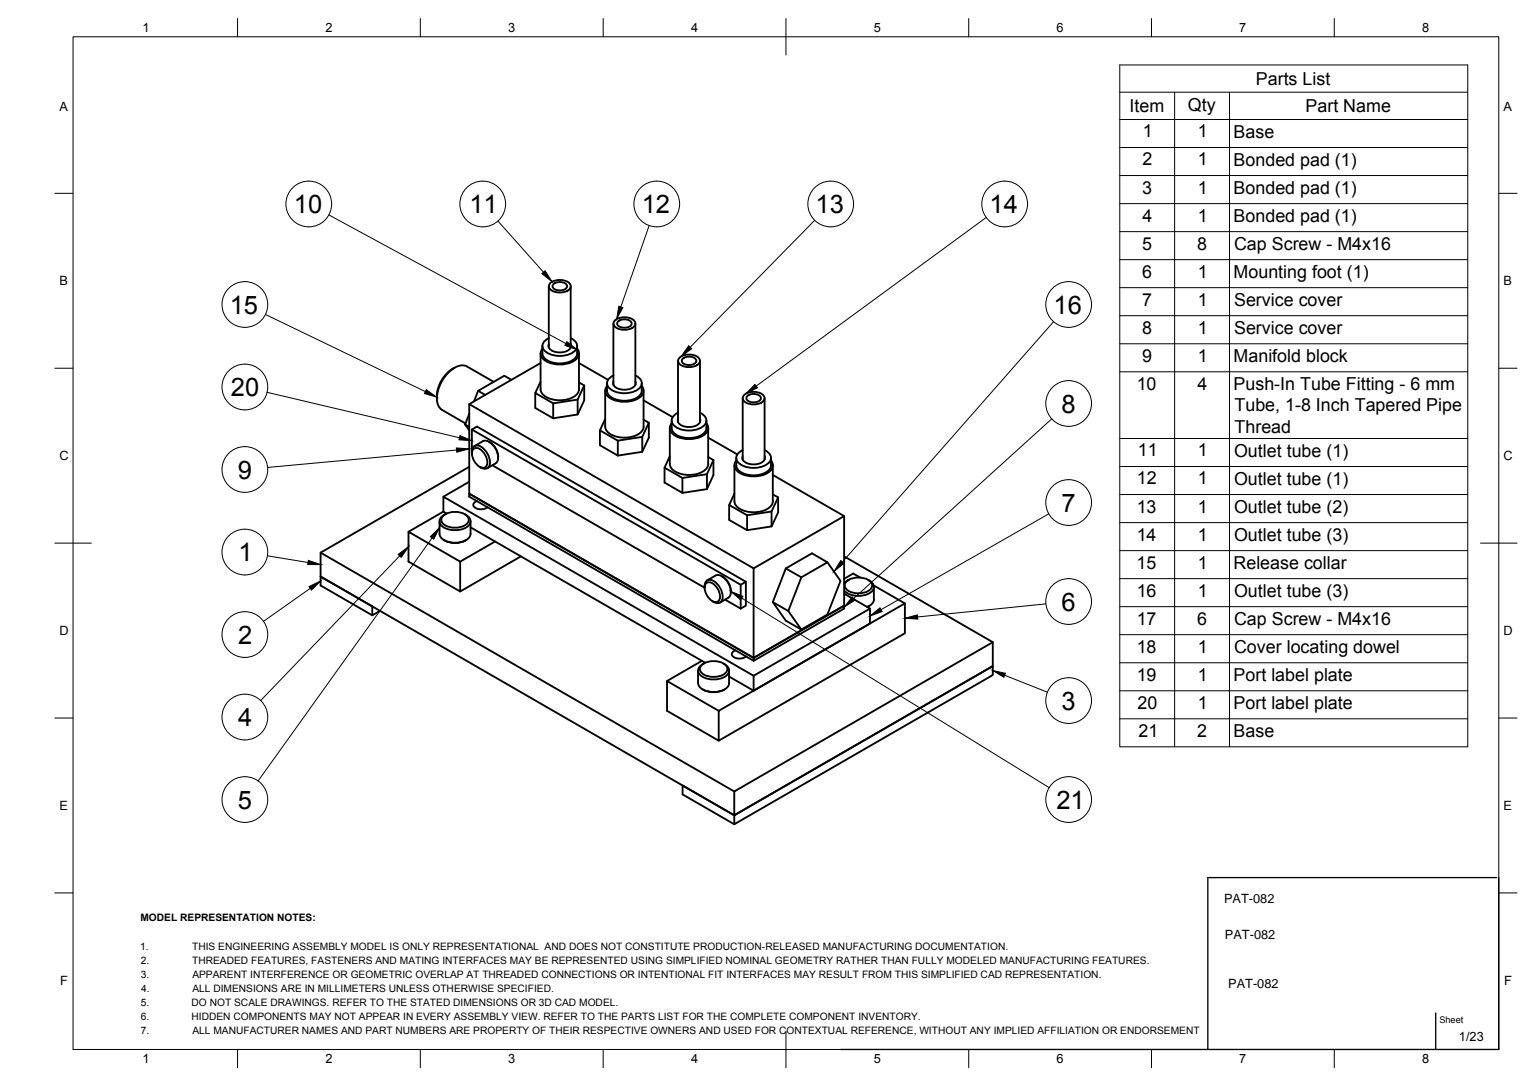
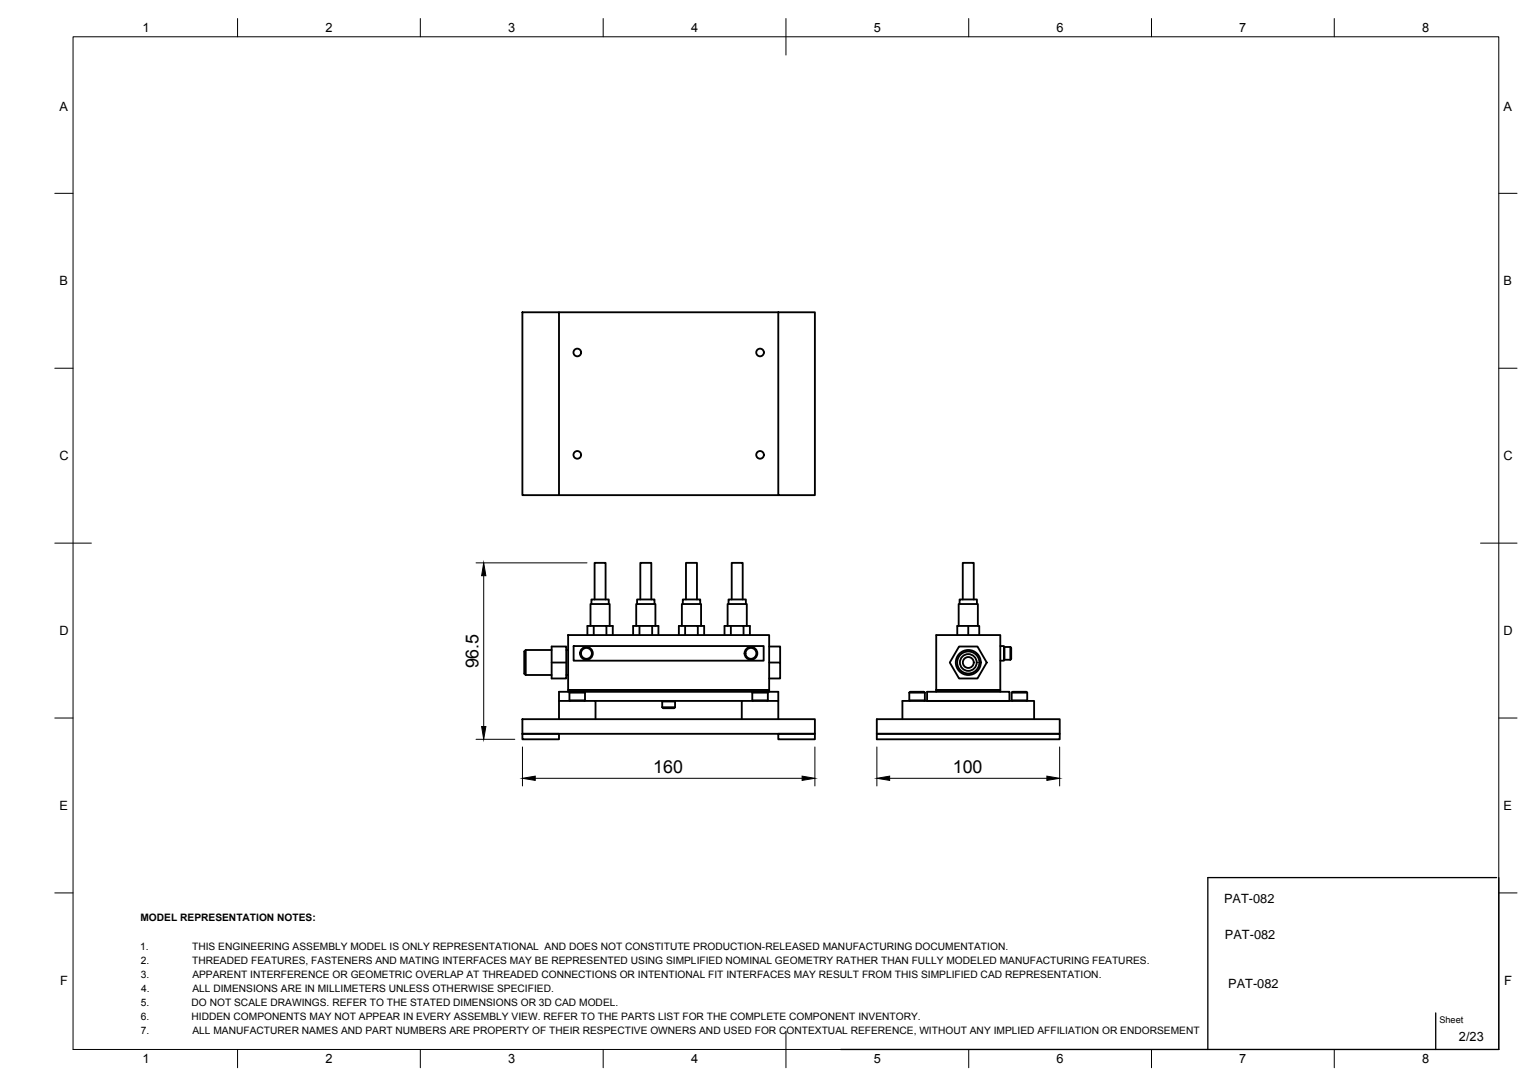
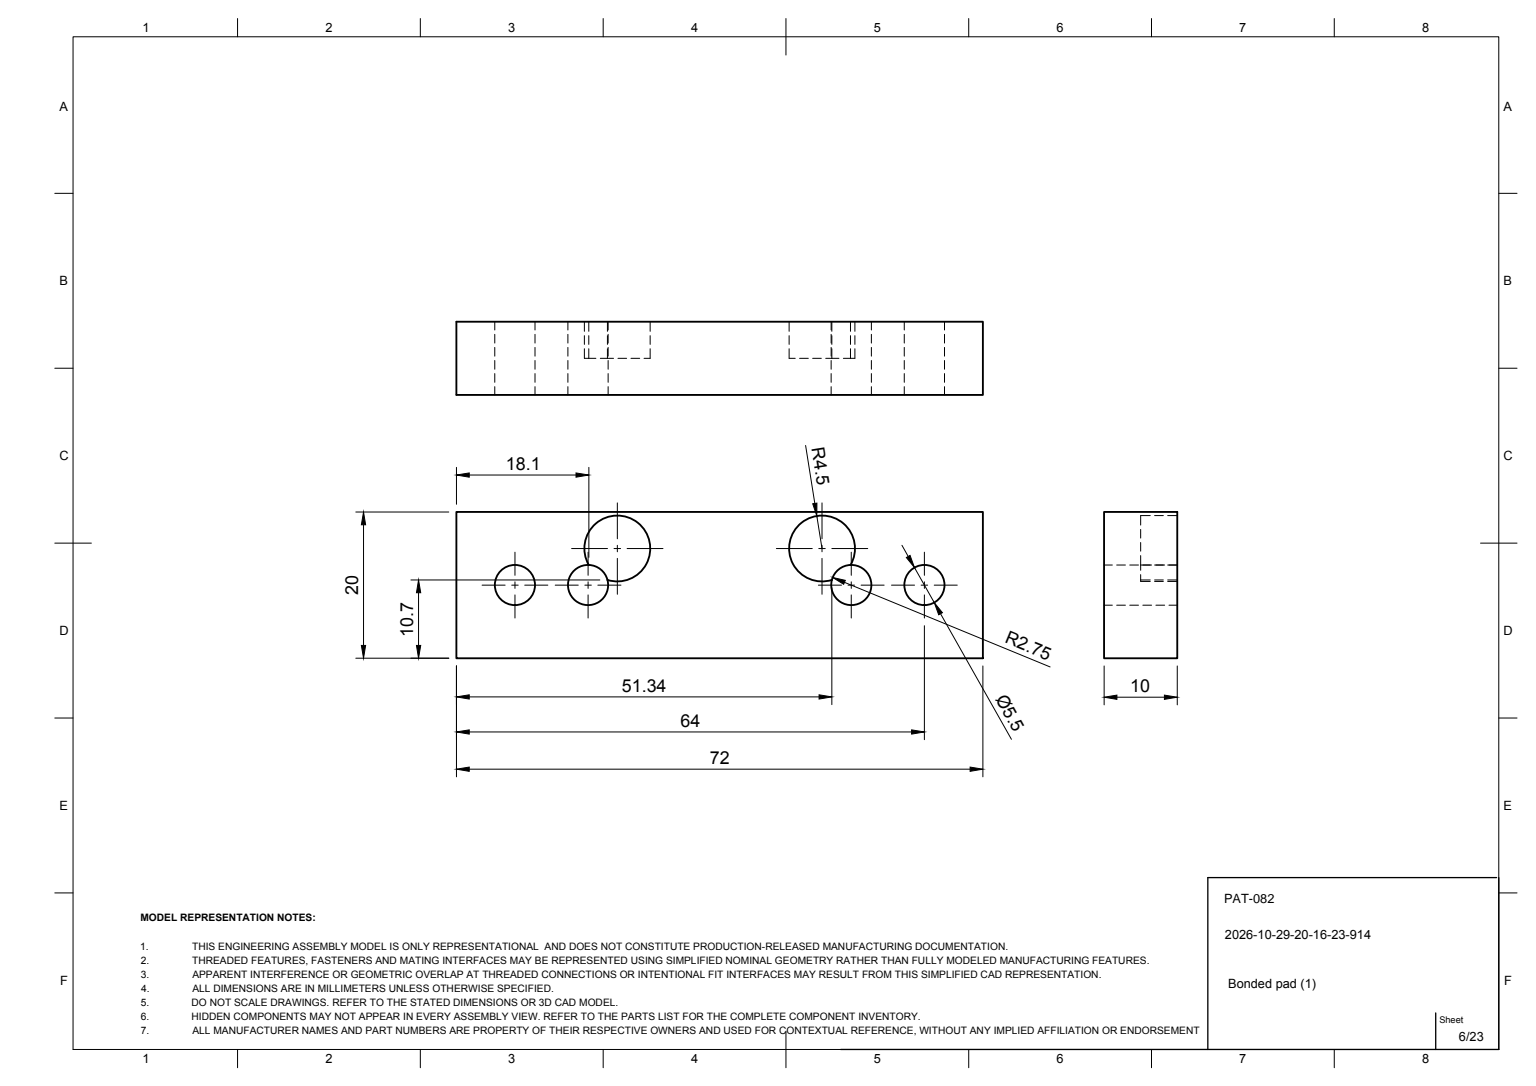
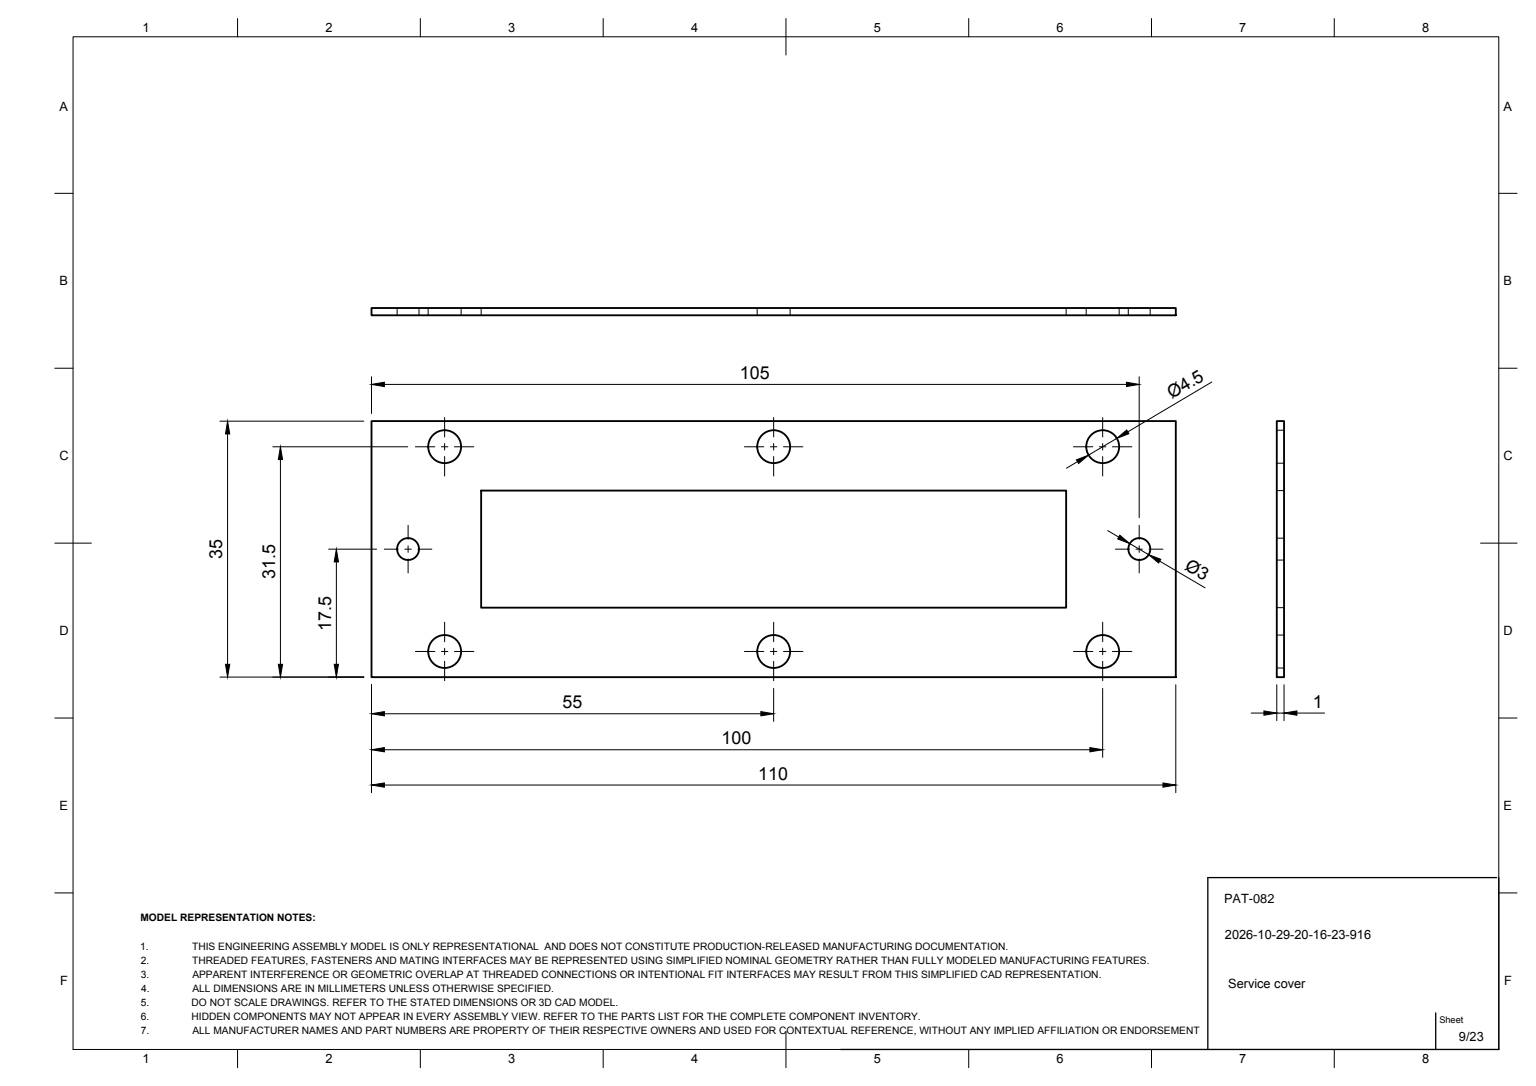
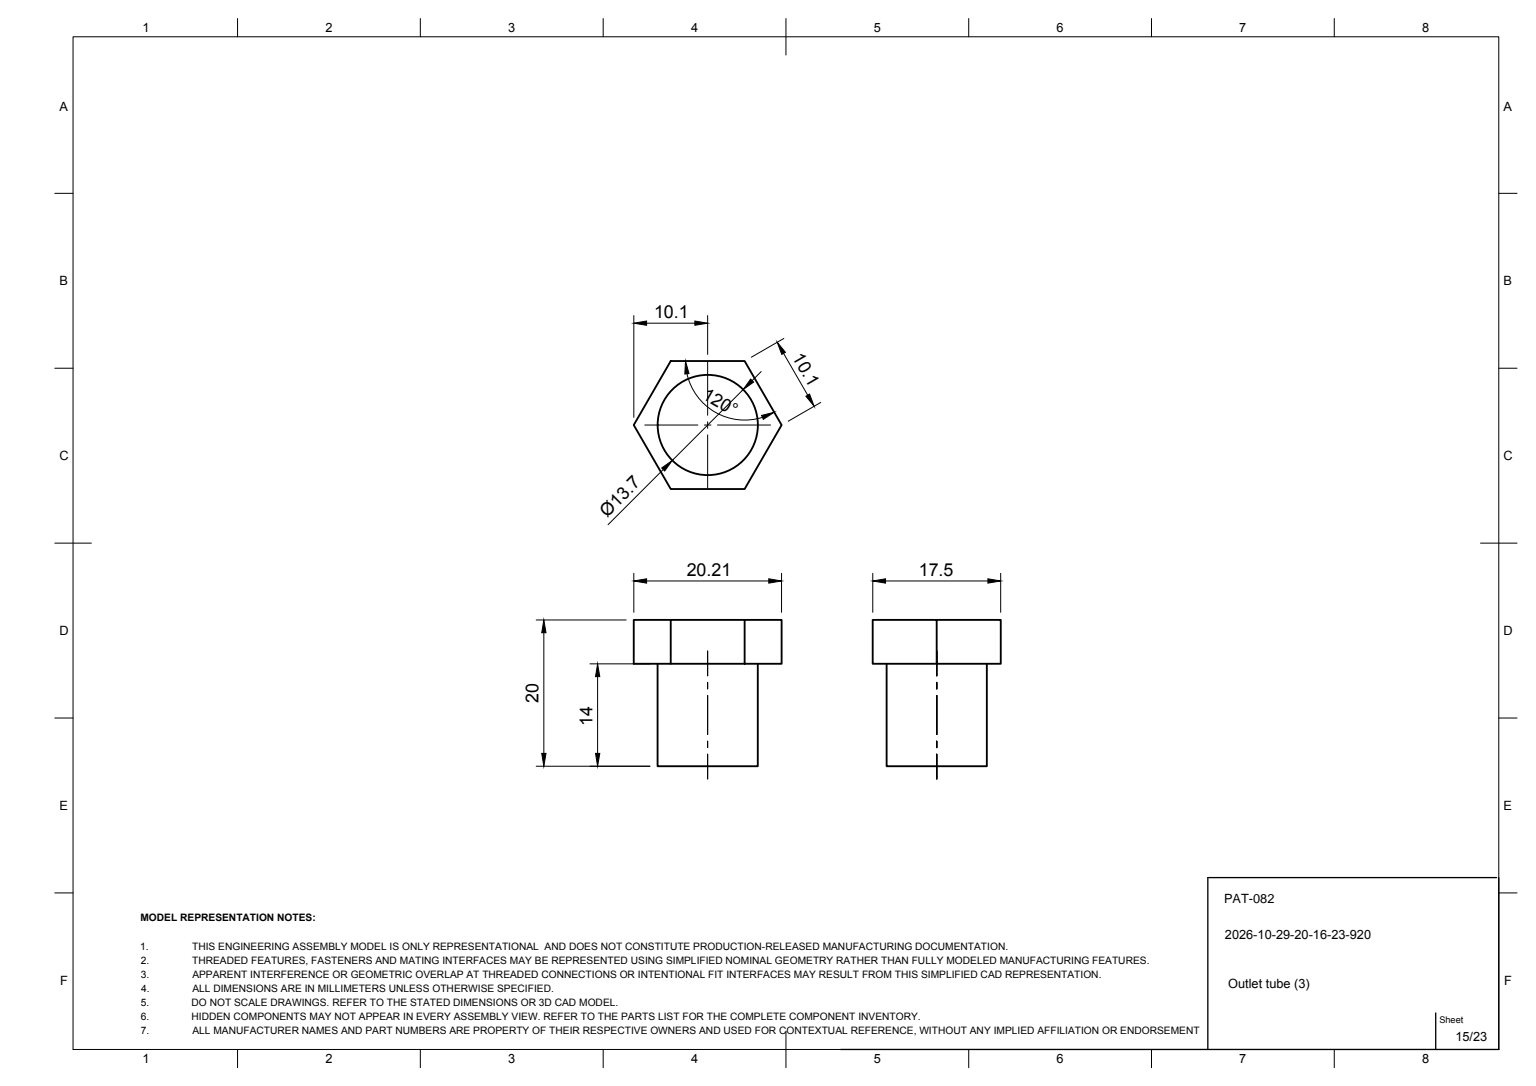
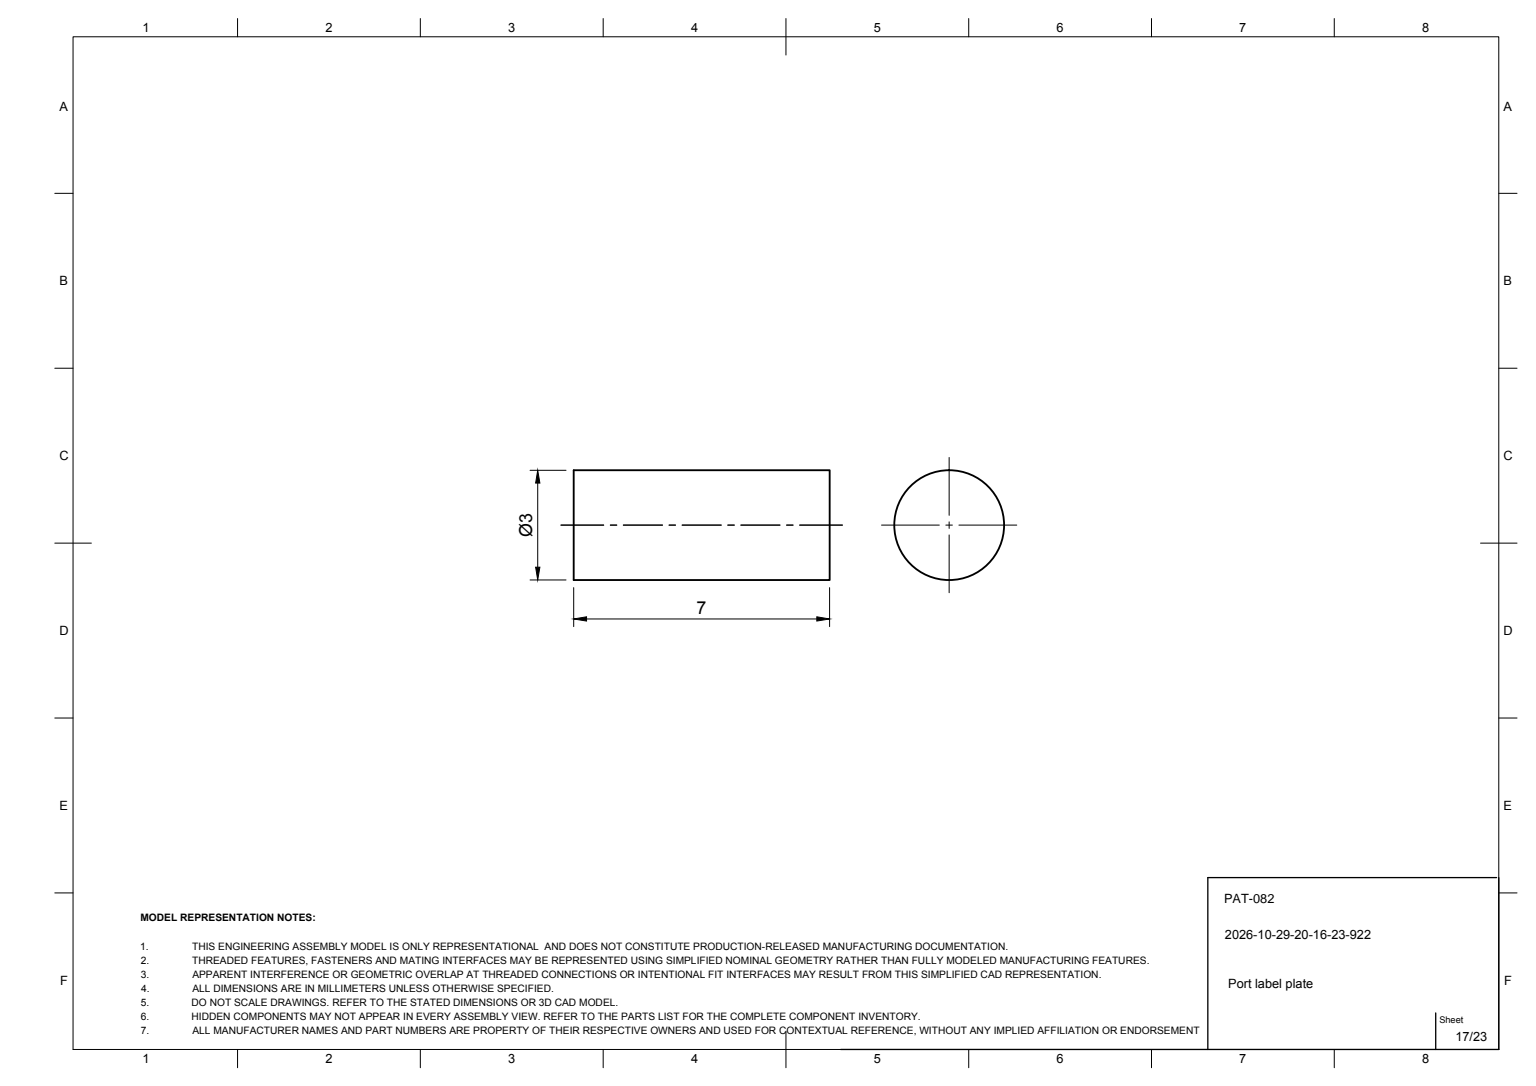
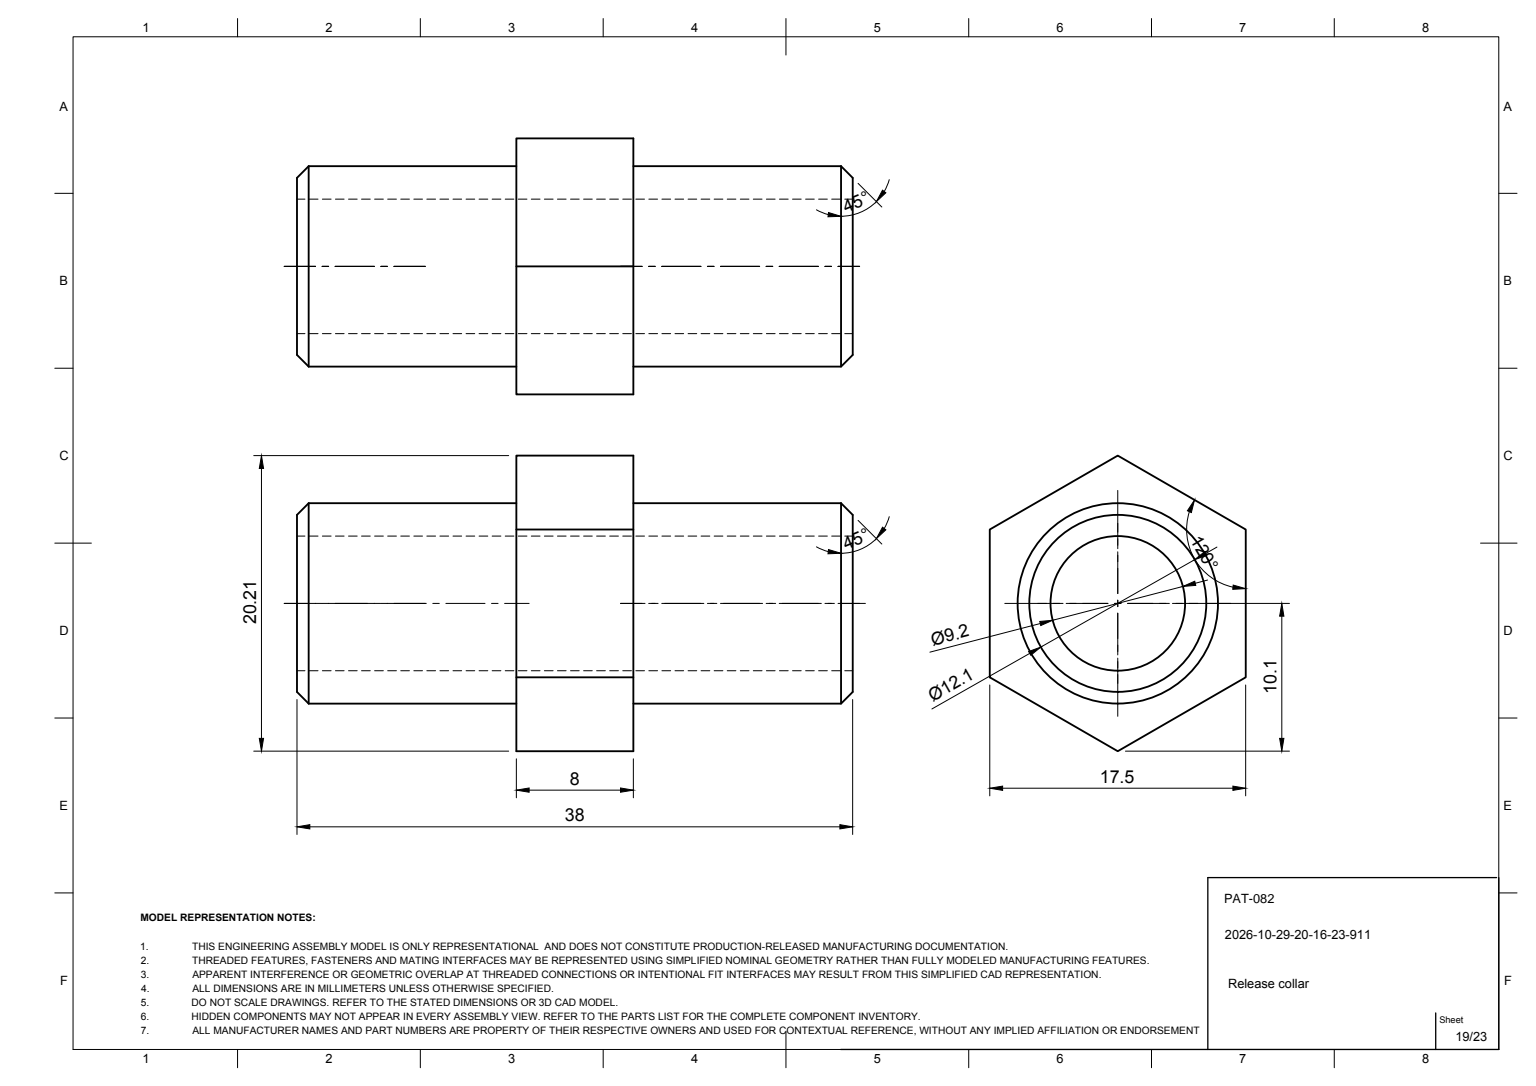
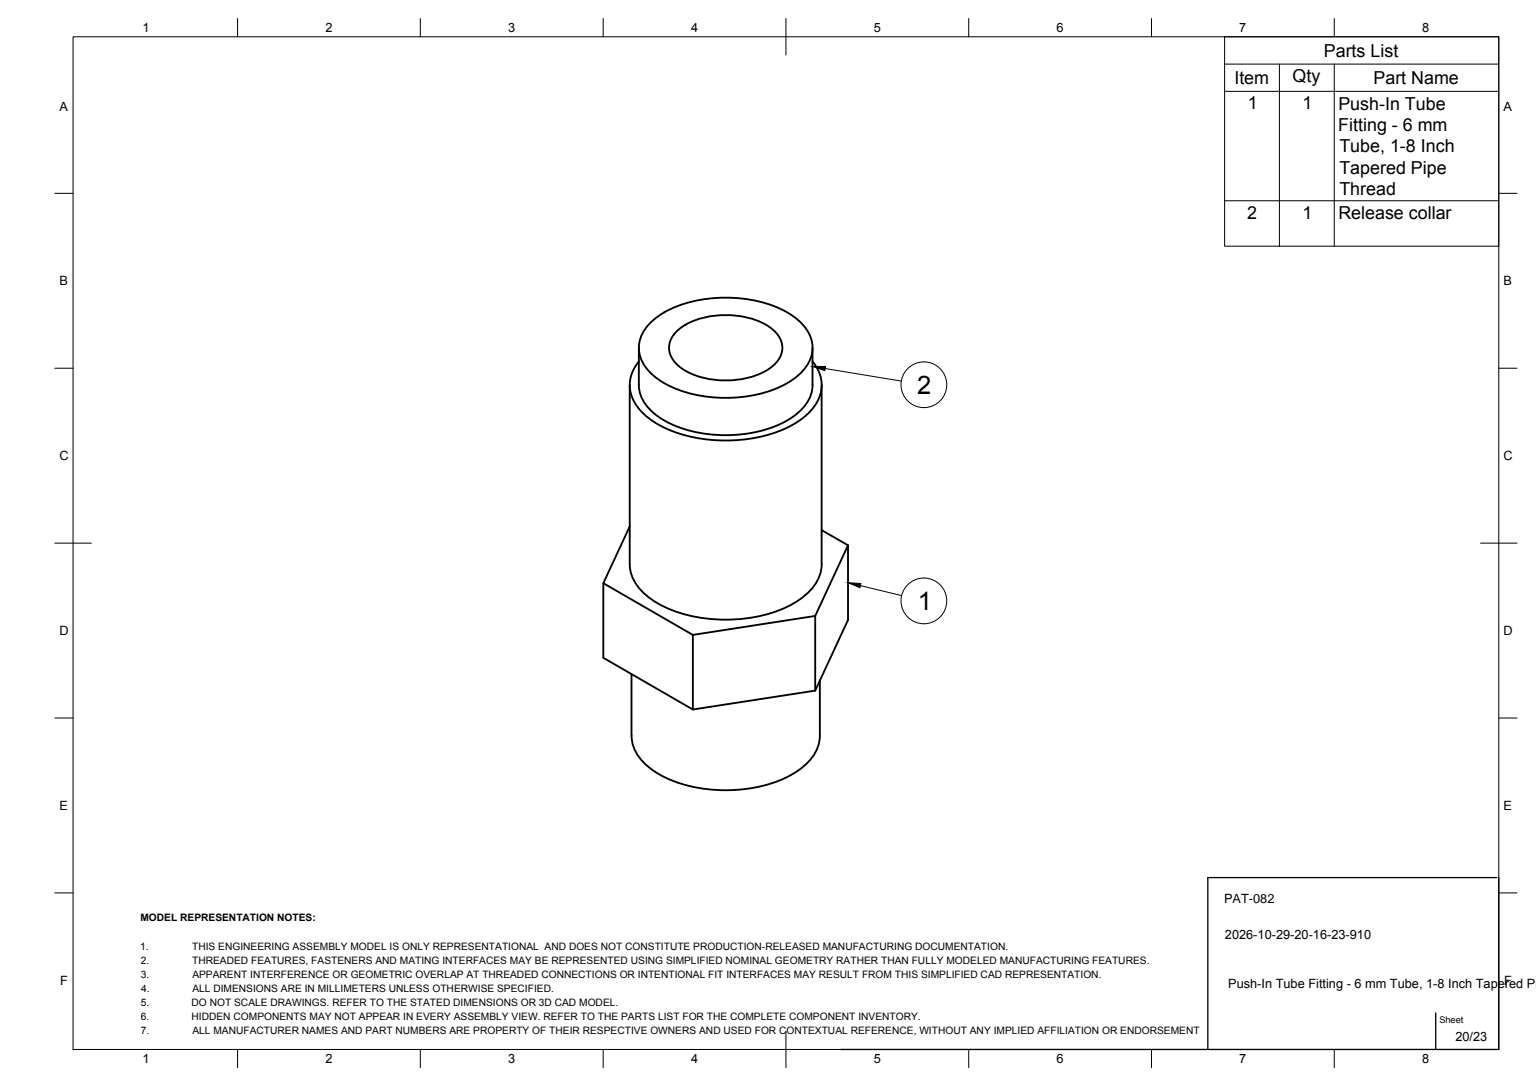
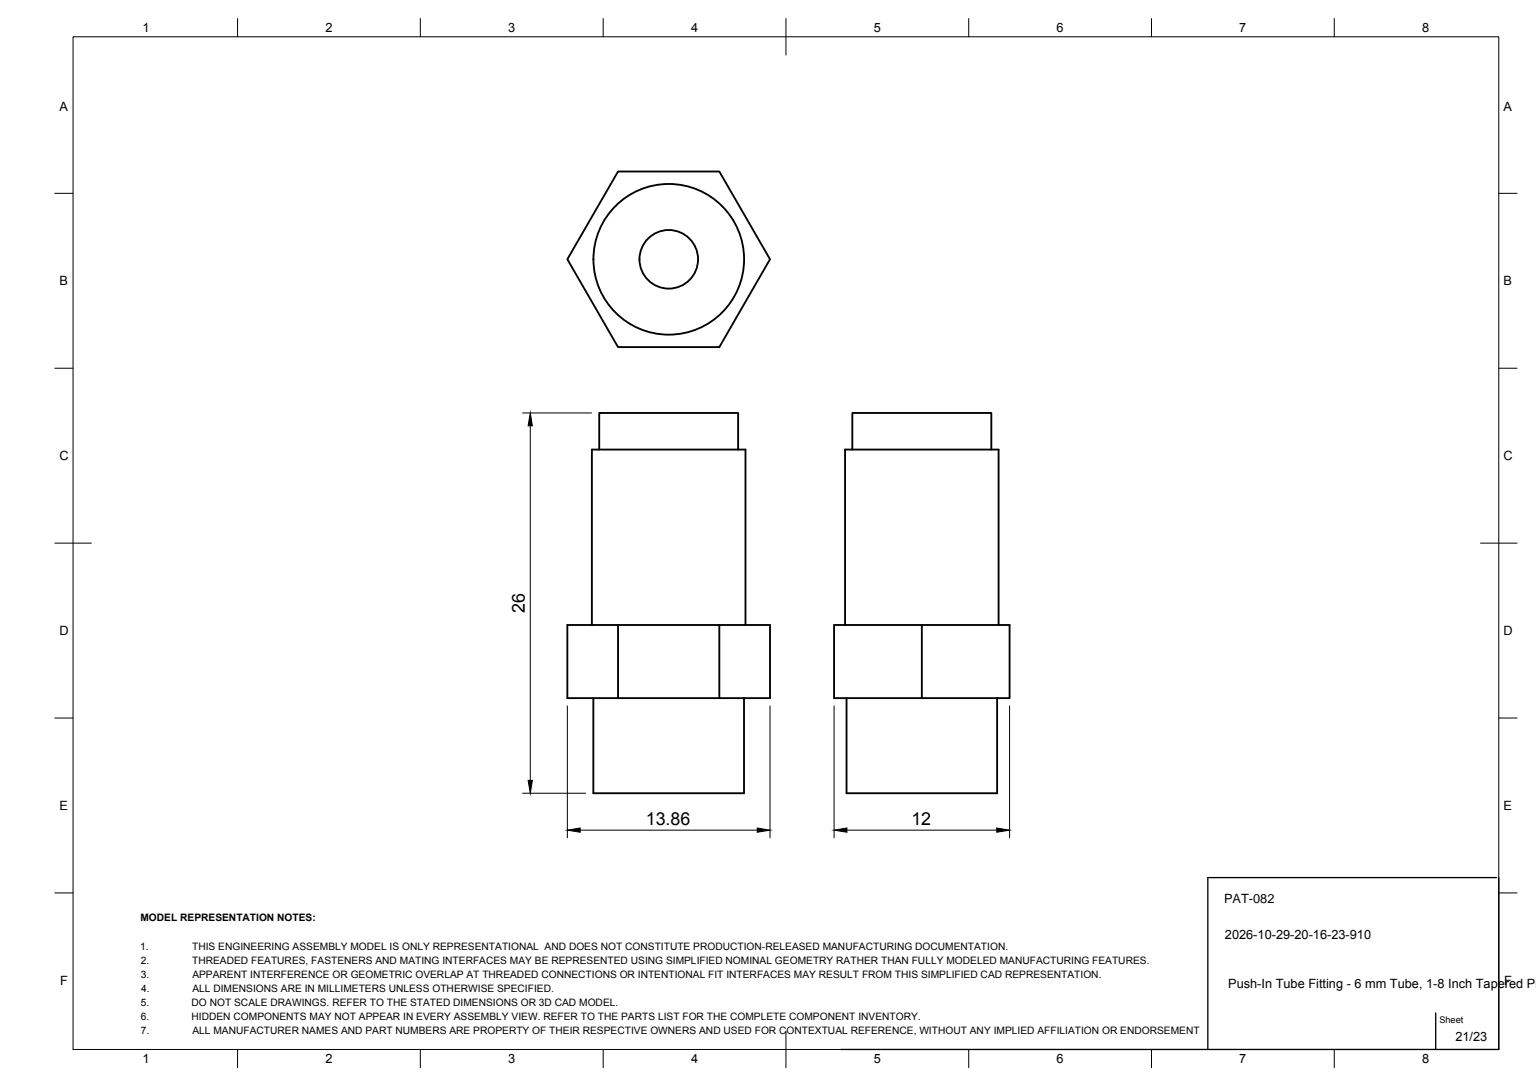
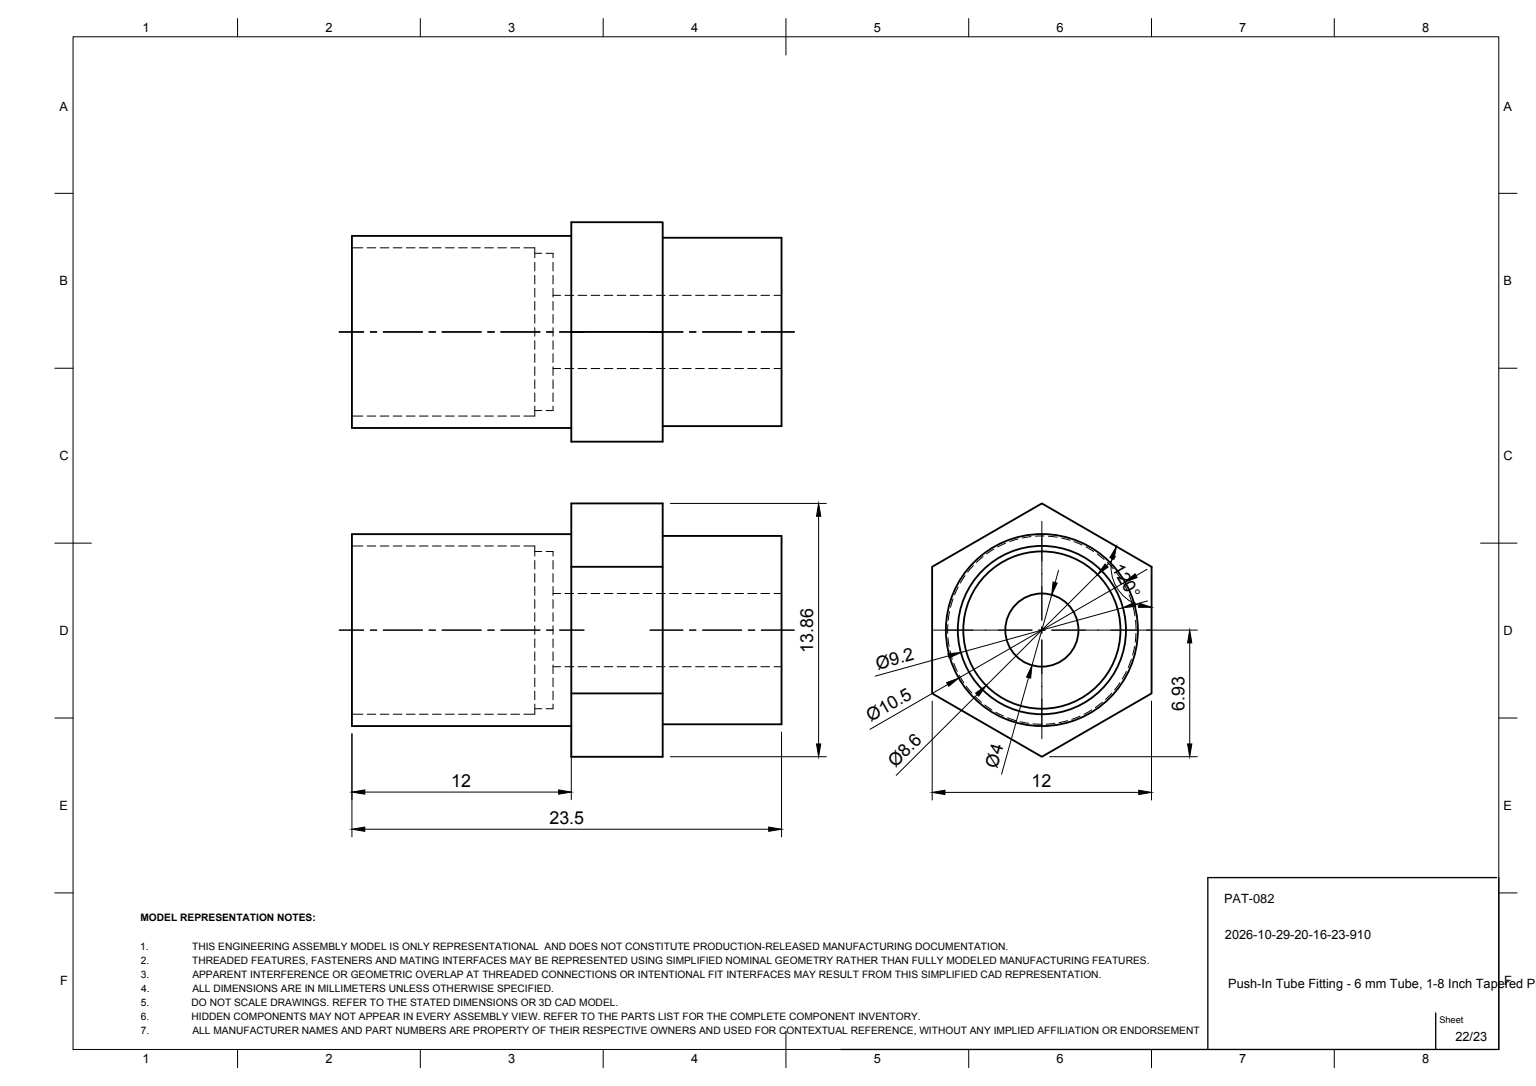
ISO-10303-21;
HEADER;
/* Generated by software containing ST-Developer
 * from STEP Tools, Inc. (www.steptools.com) 
 */

FILE_DESCRIPTION(
/* description */ ('PAT-082'),
/* implementation_level */ '2;1');

FILE_NAME(
/* name */ 'PAT-082',
/* time_stamp */ '2026-10-29T20:16:13-07:00',
/* author */ (''),
/* organization */ (''),
/* preprocessor_version */ 'ST-DEVELOPER v20.2',
/* originating_system */ 'Autodesk Translation Framework v15.17.0.0',
/* authorisation */ '');

FILE_SCHEMA (('AUTOMOTIVE_DESIGN { 1 0 10303 214 3 1 1 }'));
ENDSEC;

DATA;
#10=MECHANICAL_DESIGN_GEOMETRIC_PRESENTATION_REPRESENTATION('',(#241,#242,
#243,#244,#245,#246,#247,#248,#249,#250,#251,#252,#253,#254,#255,#256,#257,
#258,#259,#260,#261,#262),#8266);
#11=ITEM_DEFINED_TRANSFORMATION($,$,#5228,#5269);
#12=ITEM_DEFINED_TRANSFORMATION($,$,#5256,#5270);
#13=ITEM_DEFINED_TRANSFORMATION($,$,#4850,#5345);
#14=ITEM_DEFINED_TRANSFORMATION($,$,#4885,#5346);
#15=ITEM_DEFINED_TRANSFORMATION($,$,#4892,#5347);
#16=ITEM_DEFINED_TRANSFORMATION($,$,#4899,#5348);
#17=ITEM_DEFINED_TRANSFORMATION($,$,#4930,#5349);
#18=ITEM_DEFINED_TRANSFORMATION($,$,#4961,#5350);
#19=ITEM_DEFINED_TRANSFORMATION($,$,#5004,#5351);
#20=ITEM_DEFINED_TRANSFORMATION($,$,#5039,#5352);
#21=ITEM_DEFINED_TRANSFORMATION($,$,#5129,#5353);
#22=ITEM_DEFINED_TRANSFORMATION($,$,#5138,#5354);
#23=ITEM_DEFINED_TRANSFORMATION($,$,#5147,#5355);
#24=ITEM_DEFINED_TRANSFORMATION($,$,#5156,#5356);
#25=ITEM_DEFINED_TRANSFORMATION($,$,#5165,#5357);
#26=ITEM_DEFINED_TRANSFORMATION($,$,#5178,#5358);
#27=ITEM_DEFINED_TRANSFORMATION($,$,#5184,#5359);
#28=ITEM_DEFINED_TRANSFORMATION($,$,#5190,#5360);
#29=ITEM_DEFINED_TRANSFORMATION($,$,#5203,#5361);
#30=ITEM_DEFINED_TRANSFORMATION($,$,#5203,#5362);
#31=ITEM_DEFINED_TRANSFORMATION($,$,#5203,#5363);
#32=ITEM_DEFINED_TRANSFORMATION($,$,#5203,#5364);
#33=ITEM_DEFINED_TRANSFORMATION($,$,#5203,#5365);
#34=ITEM_DEFINED_TRANSFORMATION($,$,#5203,#5366);
#35=ITEM_DEFINED_TRANSFORMATION($,$,#5203,#5367);
#36=ITEM_DEFINED_TRANSFORMATION($,$,#5203,#5368);
#37=ITEM_DEFINED_TRANSFORMATION($,$,#5227,#5369);
#38=ITEM_DEFINED_TRANSFORMATION($,$,#5227,#5370);
#39=ITEM_DEFINED_TRANSFORMATION($,$,#5227,#5371);
#40=ITEM_DEFINED_TRANSFORMATION($,$,#5227,#5372);
#41=ITEM_DEFINED_TRANSFORMATION($,$,#5271,#5373);
#42=ITEM_DEFINED_TRANSFORMATION($,$,#5295,#5374);
#43=ITEM_DEFINED_TRANSFORMATION($,$,#5295,#5375);
#44=ITEM_DEFINED_TRANSFORMATION($,$,#5295,#5376);
#45=ITEM_DEFINED_TRANSFORMATION($,$,#5295,#5377);
#46=ITEM_DEFINED_TRANSFORMATION($,$,#5295,#5378);
#47=ITEM_DEFINED_TRANSFORMATION($,$,#5295,#5379);
#48=ITEM_DEFINED_TRANSFORMATION($,$,#5321,#5380);
#49=ITEM_DEFINED_TRANSFORMATION($,$,#5321,#5381);
#50=(
REPRESENTATION_RELATIONSHIP($,$,#8377,#8376)
REPRESENTATION_RELATIONSHIP_WITH_TRANSFORMATION(#11)
SHAPE_REPRESENTATION_RELATIONSHIP()
);
#51=(
REPRESENTATION_RELATIONSHIP($,$,#8378,#8376)
REPRESENTATION_RELATIONSHIP_WITH_TRANSFORMATION(#12)
SHAPE_REPRESENTATION_RELATIONSHIP()
);
#52=(
REPRESENTATION_RELATIONSHIP($,$,#8359,#8358)
REPRESENTATION_RELATIONSHIP_WITH_TRANSFORMATION(#13)
SHAPE_REPRESENTATION_RELATIONSHIP()
);
#53=(
REPRESENTATION_RELATIONSHIP($,$,#8360,#8358)
REPRESENTATION_RELATIONSHIP_WITH_TRANSFORMATION(#14)
SHAPE_REPRESENTATION_RELATIONSHIP()
);
#54=(
REPRESENTATION_RELATIONSHIP($,$,#8361,#8358)
REPRESENTATION_RELATIONSHIP_WITH_TRANSFORMATION(#15)
SHAPE_REPRESENTATION_RELATIONSHIP()
);
#55=(
REPRESENTATION_RELATIONSHIP($,$,#8362,#8358)
REPRESENTATION_RELATIONSHIP_WITH_TRANSFORMATION(#16)
SHAPE_REPRESENTATION_RELATIONSHIP()
);
#56=(
REPRESENTATION_RELATIONSHIP($,$,#8363,#8358)
REPRESENTATION_RELATIONSHIP_WITH_TRANSFORMATION(#17)
SHAPE_REPRESENTATION_RELATIONSHIP()
);
#57=(
REPRESENTATION_RELATIONSHIP($,$,#8364,#8358)
REPRESENTATION_RELATIONSHIP_WITH_TRANSFORMATION(#18)
SHAPE_REPRESENTATION_RELATIONSHIP()
);
#58=(
REPRESENTATION_RELATIONSHIP($,$,#8365,#8358)
REPRESENTATION_RELATIONSHIP_WITH_TRANSFORMATION(#19)
SHAPE_REPRESENTATION_RELATIONSHIP()
);
#59=(
REPRESENTATION_RELATIONSHIP($,$,#8366,#8358)
REPRESENTATION_RELATIONSHIP_WITH_TRANSFORMATION(#20)
SHAPE_REPRESENTATION_RELATIONSHIP()
);
#60=(
REPRESENTATION_RELATIONSHIP($,$,#8367,#8358)
REPRESENTATION_RELATIONSHIP_WITH_TRANSFORMATION(#21)
SHAPE_REPRESENTATION_RELATIONSHIP()
);
#61=(
REPRESENTATION_RELATIONSHIP($,$,#8368,#8358)
REPRESENTATION_RELATIONSHIP_WITH_TRANSFORMATION(#22)
SHAPE_REPRESENTATION_RELATIONSHIP()
);
#62=(
REPRESENTATION_RELATIONSHIP($,$,#8369,#8358)
REPRESENTATION_RELATIONSHIP_WITH_TRANSFORMATION(#23)
SHAPE_REPRESENTATION_RELATIONSHIP()
);
#63=(
REPRESENTATION_RELATIONSHIP($,$,#8370,#8358)
REPRESENTATION_RELATIONSHIP_WITH_TRANSFORMATION(#24)
SHAPE_REPRESENTATION_RELATIONSHIP()
);
#64=(
REPRESENTATION_RELATIONSHIP($,$,#8371,#8358)
REPRESENTATION_RELATIONSHIP_WITH_TRANSFORMATION(#25)
SHAPE_REPRESENTATION_RELATIONSHIP()
);
#65=(
REPRESENTATION_RELATIONSHIP($,$,#8372,#8358)
REPRESENTATION_RELATIONSHIP_WITH_TRANSFORMATION(#26)
SHAPE_REPRESENTATION_RELATIONSHIP()
);
#66=(
REPRESENTATION_RELATIONSHIP($,$,#8373,#8358)
REPRESENTATION_RELATIONSHIP_WITH_TRANSFORMATION(#27)
SHAPE_REPRESENTATION_RELATIONSHIP()
);
#67=(
REPRESENTATION_RELATIONSHIP($,$,#8374,#8358)
REPRESENTATION_RELATIONSHIP_WITH_TRANSFORMATION(#28)
SHAPE_REPRESENTATION_RELATIONSHIP()
);
#68=(
REPRESENTATION_RELATIONSHIP($,$,#8375,#8358)
REPRESENTATION_RELATIONSHIP_WITH_TRANSFORMATION(#29)
SHAPE_REPRESENTATION_RELATIONSHIP()
);
#69=(
REPRESENTATION_RELATIONSHIP($,$,#8375,#8358)
REPRESENTATION_RELATIONSHIP_WITH_TRANSFORMATION(#30)
SHAPE_REPRESENTATION_RELATIONSHIP()
);
#70=(
REPRESENTATION_RELATIONSHIP($,$,#8375,#8358)
REPRESENTATION_RELATIONSHIP_WITH_TRANSFORMATION(#31)
SHAPE_REPRESENTATION_RELATIONSHIP()
);
#71=(
REPRESENTATION_RELATIONSHIP($,$,#8375,#8358)
REPRESENTATION_RELATIONSHIP_WITH_TRANSFORMATION(#32)
SHAPE_REPRESENTATION_RELATIONSHIP()
);
#72=(
REPRESENTATION_RELATIONSHIP($,$,#8375,#8358)
REPRESENTATION_RELATIONSHIP_WITH_TRANSFORMATION(#33)
SHAPE_REPRESENTATION_RELATIONSHIP()
);
#73=(
REPRESENTATION_RELATIONSHIP($,$,#8375,#8358)
REPRESENTATION_RELATIONSHIP_WITH_TRANSFORMATION(#34)
SHAPE_REPRESENTATION_RELATIONSHIP()
);
#74=(
REPRESENTATION_RELATIONSHIP($,$,#8375,#8358)
REPRESENTATION_RELATIONSHIP_WITH_TRANSFORMATION(#35)
SHAPE_REPRESENTATION_RELATIONSHIP()
);
#75=(
REPRESENTATION_RELATIONSHIP($,$,#8375,#8358)
REPRESENTATION_RELATIONSHIP_WITH_TRANSFORMATION(#36)
SHAPE_REPRESENTATION_RELATIONSHIP()
);
#76=(
REPRESENTATION_RELATIONSHIP($,$,#8376,#8358)
REPRESENTATION_RELATIONSHIP_WITH_TRANSFORMATION(#37)
SHAPE_REPRESENTATION_RELATIONSHIP()
);
#77=(
REPRESENTATION_RELATIONSHIP($,$,#8376,#8358)
REPRESENTATION_RELATIONSHIP_WITH_TRANSFORMATION(#38)
SHAPE_REPRESENTATION_RELATIONSHIP()
);
#78=(
REPRESENTATION_RELATIONSHIP($,$,#8376,#8358)
REPRESENTATION_RELATIONSHIP_WITH_TRANSFORMATION(#39)
SHAPE_REPRESENTATION_RELATIONSHIP()
);
#79=(
REPRESENTATION_RELATIONSHIP($,$,#8376,#8358)
REPRESENTATION_RELATIONSHIP_WITH_TRANSFORMATION(#40)
SHAPE_REPRESENTATION_RELATIONSHIP()
);
#80=(
REPRESENTATION_RELATIONSHIP($,$,#8379,#8358)
REPRESENTATION_RELATIONSHIP_WITH_TRANSFORMATION(#41)
SHAPE_REPRESENTATION_RELATIONSHIP()
);
#81=(
REPRESENTATION_RELATIONSHIP($,$,#8380,#8358)
REPRESENTATION_RELATIONSHIP_WITH_TRANSFORMATION(#42)
SHAPE_REPRESENTATION_RELATIONSHIP()
);
#82=(
REPRESENTATION_RELATIONSHIP($,$,#8380,#8358)
REPRESENTATION_RELATIONSHIP_WITH_TRANSFORMATION(#43)
SHAPE_REPRESENTATION_RELATIONSHIP()
);
#83=(
REPRESENTATION_RELATIONSHIP($,$,#8380,#8358)
REPRESENTATION_RELATIONSHIP_WITH_TRANSFORMATION(#44)
SHAPE_REPRESENTATION_RELATIONSHIP()
);
#84=(
REPRESENTATION_RELATIONSHIP($,$,#8380,#8358)
REPRESENTATION_RELATIONSHIP_WITH_TRANSFORMATION(#45)
SHAPE_REPRESENTATION_RELATIONSHIP()
);
#85=(
REPRESENTATION_RELATIONSHIP($,$,#8380,#8358)
REPRESENTATION_RELATIONSHIP_WITH_TRANSFORMATION(#46)
SHAPE_REPRESENTATION_RELATIONSHIP()
);
#86=(
REPRESENTATION_RELATIONSHIP($,$,#8380,#8358)
REPRESENTATION_RELATIONSHIP_WITH_TRANSFORMATION(#47)
SHAPE_REPRESENTATION_RELATIONSHIP()
);
#87=(
REPRESENTATION_RELATIONSHIP($,$,#8381,#8358)
REPRESENTATION_RELATIONSHIP_WITH_TRANSFORMATION(#48)
SHAPE_REPRESENTATION_RELATIONSHIP()
);
#88=(
REPRESENTATION_RELATIONSHIP($,$,#8381,#8358)
REPRESENTATION_RELATIONSHIP_WITH_TRANSFORMATION(#49)
SHAPE_REPRESENTATION_RELATIONSHIP()
);
#89=CONTEXT_DEPENDENT_SHAPE_REPRESENTATION(#50,#8316);
#90=CONTEXT_DEPENDENT_SHAPE_REPRESENTATION(#51,#8317);
#91=CONTEXT_DEPENDENT_SHAPE_REPRESENTATION(#52,#8321);
#92=CONTEXT_DEPENDENT_SHAPE_REPRESENTATION(#53,#8322);
#93=CONTEXT_DEPENDENT_SHAPE_REPRESENTATION(#54,#8323);
#94=CONTEXT_DEPENDENT_SHAPE_REPRESENTATION(#55,#8324);
#95=CONTEXT_DEPENDENT_SHAPE_REPRESENTATION(#56,#8325);
#96=CONTEXT_DEPENDENT_SHAPE_REPRESENTATION(#57,#8326);
#97=CONTEXT_DEPENDENT_SHAPE_REPRESENTATION(#58,#8327);
#98=CONTEXT_DEPENDENT_SHAPE_REPRESENTATION(#59,#8328);
#99=CONTEXT_DEPENDENT_SHAPE_REPRESENTATION(#60,#8329);
#100=CONTEXT_DEPENDENT_SHAPE_REPRESENTATION(#61,#8330);
#101=CONTEXT_DEPENDENT_SHAPE_REPRESENTATION(#62,#8331);
#102=CONTEXT_DEPENDENT_SHAPE_REPRESENTATION(#63,#8332);
#103=CONTEXT_DEPENDENT_SHAPE_REPRESENTATION(#64,#8333);
#104=CONTEXT_DEPENDENT_SHAPE_REPRESENTATION(#65,#8334);
#105=CONTEXT_DEPENDENT_SHAPE_REPRESENTATION(#66,#8335);
#106=CONTEXT_DEPENDENT_SHAPE_REPRESENTATION(#67,#8336);
#107=CONTEXT_DEPENDENT_SHAPE_REPRESENTATION(#68,#8337);
#108=CONTEXT_DEPENDENT_SHAPE_REPRESENTATION(#69,#8338);
#109=CONTEXT_DEPENDENT_SHAPE_REPRESENTATION(#70,#8339);
#110=CONTEXT_DEPENDENT_SHAPE_REPRESENTATION(#71,#8340);
#111=CONTEXT_DEPENDENT_SHAPE_REPRESENTATION(#72,#8341);
#112=CONTEXT_DEPENDENT_SHAPE_REPRESENTATION(#73,#8342);
#113=CONTEXT_DEPENDENT_SHAPE_REPRESENTATION(#74,#8343);
#114=CONTEXT_DEPENDENT_SHAPE_REPRESENTATION(#75,#8344);
#115=CONTEXT_DEPENDENT_SHAPE_REPRESENTATION(#76,#8345);
#116=CONTEXT_DEPENDENT_SHAPE_REPRESENTATION(#77,#8346);
#117=CONTEXT_DEPENDENT_SHAPE_REPRESENTATION(#78,#8347);
#118=CONTEXT_DEPENDENT_SHAPE_REPRESENTATION(#79,#8348);
#119=CONTEXT_DEPENDENT_SHAPE_REPRESENTATION(#80,#8349);
#120=CONTEXT_DEPENDENT_SHAPE_REPRESENTATION(#81,#8350);
#121=CONTEXT_DEPENDENT_SHAPE_REPRESENTATION(#82,#8351);
#122=CONTEXT_DEPENDENT_SHAPE_REPRESENTATION(#83,#8352);
#123=CONTEXT_DEPENDENT_SHAPE_REPRESENTATION(#84,#8353);
#124=CONTEXT_DEPENDENT_SHAPE_REPRESENTATION(#85,#8354);
#125=CONTEXT_DEPENDENT_SHAPE_REPRESENTATION(#86,#8355);
#126=CONTEXT_DEPENDENT_SHAPE_REPRESENTATION(#87,#8356);
#127=CONTEXT_DEPENDENT_SHAPE_REPRESENTATION(#88,#8357);
#128=NEXT_ASSEMBLY_USAGE_OCCURRENCE('Body:1','Body:1','Body:1',#8401,#8402,
'Body:1');
#129=NEXT_ASSEMBLY_USAGE_OCCURRENCE('Release collar:1',
'Release collar:1','Release collar:1',#8401,#8403,'Release collar:1');
#130=NEXT_ASSEMBLY_USAGE_OCCURRENCE('Base:1','Base:1','Base:1',#8383,#8384,
'Base:1');
#131=NEXT_ASSEMBLY_USAGE_OCCURRENCE('Bonded pad:1','Bonded pad:1',
'Bonded pad:1',#8383,#8385,'Bonded pad:1');
#132=NEXT_ASSEMBLY_USAGE_OCCURRENCE('Bonded pad (1):1',
'Bonded pad (1):1','Bonded pad (1):1',#8383,#8386,'Bonded pad (1):1');
#133=NEXT_ASSEMBLY_USAGE_OCCURRENCE('Mounting foot:1','Mounting foot:1',
'Mounting foot:1',#8383,#8387,'Mounting foot:1');
#134=NEXT_ASSEMBLY_USAGE_OCCURRENCE('Mounting foot (1):1',
'Mounting foot (1):1','Mounting foot (1):1',#8383,#8388,
'Mounting foot (1):1');
#135=NEXT_ASSEMBLY_USAGE_OCCURRENCE('Service cover:1','Service cover:1',
'Service cover:1',#8383,#8389,'Service cover:1');
#136=NEXT_ASSEMBLY_USAGE_OCCURRENCE('Cover gasket:1','Cover gasket:1',
'Cover gasket:1',#8383,#8390,'Cover gasket:1');
#137=NEXT_ASSEMBLY_USAGE_OCCURRENCE('Manifold block:1',
'Manifold block:1','Manifold block:1',#8383,#8391,'Manifold block:1');
#138=NEXT_ASSEMBLY_USAGE_OCCURRENCE('Outlet tube:1','Outlet tube:1',
'Outlet tube:1',#8383,#8392,'Outlet tube:1');
#139=NEXT_ASSEMBLY_USAGE_OCCURRENCE('Outlet tube (1):1',
'Outlet tube (1):1','Outlet tube (1):1',#8383,#8393,'Outlet tube (1):1');
#140=NEXT_ASSEMBLY_USAGE_OCCURRENCE('Outlet tube (2):1',
'Outlet tube (2):1','Outlet tube (2):1',#8383,#8394,'Outlet tube (2):1');
#141=NEXT_ASSEMBLY_USAGE_OCCURRENCE('Outlet tube (3):1',
'Outlet tube (3):1','Outlet tube (3):1',#8383,#8395,'Outlet tube (3):1');
#142=NEXT_ASSEMBLY_USAGE_OCCURRENCE('Blanking plug:1','Blanking plug:1',
'Blanking plug:1',#8383,#8396,'Blanking plug:1');
#143=NEXT_ASSEMBLY_USAGE_OCCURRENCE('Cover locating dowel:1',
'Cover locating dowel:1','Cover locating dowel:1',#8383,#8397,
'Cover locating dowel:1');
#144=NEXT_ASSEMBLY_USAGE_OCCURRENCE('Cover locating dowel (1):1',
'Cover locating dowel (1):1','Cover locating dowel (1):1',#8383,#8398,
'Cover locating dowel (1):1');
#145=NEXT_ASSEMBLY_USAGE_OCCURRENCE('Port label plate:1',
'Port label plate:1','Port label plate:1',#8383,#8399,
'Port label plate:1');
#146=NEXT_ASSEMBLY_USAGE_OCCURRENCE('M5x14 Cap Screw:1',
'M5x14 Cap Screw:1','M5x14 Cap Screw:1',#8383,#8400,'M5x14 Cap Screw:1');
#147=NEXT_ASSEMBLY_USAGE_OCCURRENCE('M5x14 Cap Screw:2',
'M5x14 Cap Screw:2','M5x14 Cap Screw:2',#8383,#8400,'M5x14 Cap Screw:2');
#148=NEXT_ASSEMBLY_USAGE_OCCURRENCE('M5x14 Cap Screw:3',
'M5x14 Cap Screw:3','M5x14 Cap Screw:3',#8383,#8400,'M5x14 Cap Screw:3');
#149=NEXT_ASSEMBLY_USAGE_OCCURRENCE('M5x14 Cap Screw:4',
'M5x14 Cap Screw:4','M5x14 Cap Screw:4',#8383,#8400,'M5x14 Cap Screw:4');
#150=NEXT_ASSEMBLY_USAGE_OCCURRENCE('M5x14 Cap Screw:5',
'M5x14 Cap Screw:5','M5x14 Cap Screw:5',#8383,#8400,'M5x14 Cap Screw:5');
#151=NEXT_ASSEMBLY_USAGE_OCCURRENCE('M5x14 Cap Screw:6',
'M5x14 Cap Screw:6','M5x14 Cap Screw:6',#8383,#8400,'M5x14 Cap Screw:6');
#152=NEXT_ASSEMBLY_USAGE_OCCURRENCE('M5x14 Cap Screw:7',
'M5x14 Cap Screw:7','M5x14 Cap Screw:7',#8383,#8400,'M5x14 Cap Screw:7');
#153=NEXT_ASSEMBLY_USAGE_OCCURRENCE('M5x14 Cap Screw:8',
'M5x14 Cap Screw:8','M5x14 Cap Screw:8',#8383,#8400,'M5x14 Cap Screw:8');
#154=NEXT_ASSEMBLY_USAGE_OCCURRENCE(
'Push-In Tube Fitting - 6 mm Tube, 1-8 Inch Tapered Pipe Thread:1',
'Push-In Tube Fitting - 6 mm Tube, 1-8 Inch Tapered Pipe Thread:1',
'Push-In Tube Fitting - 6 mm Tube, 1-8 Inch Tapered Pipe Thread:1',#8383,
#8401,
'Push-In Tube Fitting - 6 mm Tube, 1-8 Inch Tapered Pipe Thread:1');
#155=NEXT_ASSEMBLY_USAGE_OCCURRENCE(
'Push-In Tube Fitting - 6 mm Tube, 1-8 Inch Tapered Pipe Thread:2',
'Push-In Tube Fitting - 6 mm Tube, 1-8 Inch Tapered Pipe Thread:2',
'Push-In Tube Fitting - 6 mm Tube, 1-8 Inch Tapered Pipe Thread:2',#8383,
#8401,
'Push-In Tube Fitting - 6 mm Tube, 1-8 Inch Tapered Pipe Thread:2');
#156=NEXT_ASSEMBLY_USAGE_OCCURRENCE(
'Push-In Tube Fitting - 6 mm Tube, 1-8 Inch Tapered Pipe Thread:3',
'Push-In Tube Fitting - 6 mm Tube, 1-8 Inch Tapered Pipe Thread:3',
'Push-In Tube Fitting - 6 mm Tube, 1-8 Inch Tapered Pipe Thread:3',#8383,
#8401,
'Push-In Tube Fitting - 6 mm Tube, 1-8 Inch Tapered Pipe Thread:3');
#157=NEXT_ASSEMBLY_USAGE_OCCURRENCE(
'Push-In Tube Fitting - 6 mm Tube, 1-8 Inch Tapered Pipe Thread:4',
'Push-In Tube Fitting - 6 mm Tube, 1-8 Inch Tapered Pipe Thread:4',
'Push-In Tube Fitting - 6 mm Tube, 1-8 Inch Tapered Pipe Thread:4',#8383,
#8401,
'Push-In Tube Fitting - 6 mm Tube, 1-8 Inch Tapered Pipe Thread:4');
#158=NEXT_ASSEMBLY_USAGE_OCCURRENCE(
'Hex Pipe Nipple - 1-4 Inch Tapered Pipe Thread:1',
'Hex Pipe Nipple - 1-4 Inch Tapered Pipe Thread:1',
'Hex Pipe Nipple - 1-4 Inch Tapered Pipe Thread:1',#8383,#8404,
'Hex Pipe Nipple - 1-4 Inch Tapered Pipe Thread:1');
#159=NEXT_ASSEMBLY_USAGE_OCCURRENCE('Cap Screw - M4x16:1',
'Cap Screw - M4x16:1','Cap Screw - M4x16:1',#8383,#8405,
'Cap Screw - M4x16:1');
#160=NEXT_ASSEMBLY_USAGE_OCCURRENCE('Cap Screw - M4x16:2',
'Cap Screw - M4x16:2','Cap Screw - M4x16:2',#8383,#8405,
'Cap Screw - M4x16:2');
#161=NEXT_ASSEMBLY_USAGE_OCCURRENCE('Cap Screw - M4x16:3',
'Cap Screw - M4x16:3','Cap Screw - M4x16:3',#8383,#8405,
'Cap Screw - M4x16:3');
#162=NEXT_ASSEMBLY_USAGE_OCCURRENCE('Cap Screw - M4x16:4',
'Cap Screw - M4x16:4','Cap Screw - M4x16:4',#8383,#8405,
'Cap Screw - M4x16:4');
#163=NEXT_ASSEMBLY_USAGE_OCCURRENCE('Cap Screw - M4x16:5',
'Cap Screw - M4x16:5','Cap Screw - M4x16:5',#8383,#8405,
'Cap Screw - M4x16:5');
#164=NEXT_ASSEMBLY_USAGE_OCCURRENCE('Cap Screw - M4x16:6',
'Cap Screw - M4x16:6','Cap Screw - M4x16:6',#8383,#8405,
'Cap Screw - M4x16:6');
#165=NEXT_ASSEMBLY_USAGE_OCCURRENCE('M4x10 Cap Screw:1',
'M4x10 Cap Screw:1','M4x10 Cap Screw:1',#8383,#8406,'M4x10 Cap Screw:1');
#166=NEXT_ASSEMBLY_USAGE_OCCURRENCE('M4x10 Cap Screw:2',
'M4x10 Cap Screw:2','M4x10 Cap Screw:2',#8383,#8406,'M4x10 Cap Screw:2');
#167=CONICAL_SURFACE('',#5216,0.4,0.785398163397448);
#168=CONICAL_SURFACE('',#5220,0.41,0.785398163397448);
#169=CONICAL_SURFACE('',#5224,0.26,0.463647609000806);
#170=CONICAL_SURFACE('',#5287,0.645,0.785398163397448);
#171=CONICAL_SURFACE('',#5290,0.645,0.785398163397448);
#172=CONICAL_SURFACE('',#5298,0.325,0.785398163397448);
#173=CONICAL_SURFACE('',#5302,0.335,0.785398163397448);
#174=CONICAL_SURFACE('',#5306,0.21,0.463647609000806);
#175=CONICAL_SURFACE('',#5310,0.18,0.785398163397448);
#176=CONICAL_SURFACE('',#5334,0.325,0.785398163397448);
#177=CONICAL_SURFACE('',#5338,0.335,0.785398163397448);
#178=CONICAL_SURFACE('',#5342,0.21,0.463647609000806);
#179=ORIENTED_CLOSED_SHELL('',*,#4597,.F.);
#180=ORIENTED_CLOSED_SHELL('',*,#4603,.F.);
#181=ORIENTED_CLOSED_SHELL('',*,#4604,.F.);
#182=BREP_WITH_VOIDS('Body1',#4598,(#179));
#183=BREP_WITH_VOIDS('Body1',#4602,(#180));
#184=BREP_WITH_VOIDS('Body1',#4605,(#181));
#185=B_SPLINE_CURVE_WITH_KNOTS('',3,(#7377,#7378,#7379,#7380,#7381,#7382,
#7383,#7384,#7385,#7386),.UNSPECIFIED.,.F.,.F.,(4,2,2,2,4),(0.,0.0789054703932598,
0.15781094078652,0.235848341776527,0.313885742766535),.UNSPECIFIED.);
#186=B_SPLINE_CURVE_WITH_KNOTS('',3,(#7388,#7389,#7390,#7391,#7392,#7393,
#7394,#7395,#7396,#7397),.UNSPECIFIED.,.F.,.F.,(4,2,2,2,4),(0.941657228299606,
1.01969462928961,1.09773203027962,1.17663750067288,1.25554297106614),
 .UNSPECIFIED.);
#187=B_SPLINE_CURVE_WITH_KNOTS('',3,(#7401,#7402,#7403,#7404,#7405,#7406,
#7407,#7408,#7409,#7410,#7411,#7412,#7413,#7414,#7415,#7416,#7417,#7418),
 .UNSPECIFIED.,.F.,.F.,(4,2,2,2,2,2,2,2,4),(0.313885742766535,0.391923143756543,
0.469960544746551,0.548866015139811,0.627771485533071,0.70667695592633,
0.78558242631959,0.863619827309598,0.941657228299606),.UNSPECIFIED.);
#188=B_SPLINE_CURVE_WITH_KNOTS('',3,(#7429,#7430,#7431,#7432,#7433,#7434,
#7435,#7436,#7437,#7438),.UNSPECIFIED.,.F.,.F.,(4,2,2,2,4),(0.,0.0789054703932594,
0.157810940786519,0.235848341776527,0.313885742766535),.UNSPECIFIED.);
#189=B_SPLINE_CURVE_WITH_KNOTS('',3,(#7440,#7441,#7442,#7443,#7444,#7445,
#7446,#7447,#7448,#7449),.UNSPECIFIED.,.F.,.F.,(4,2,2,2,4),(0.941657228299605,
1.01969462928961,1.09773203027962,1.17663750067288,1.25554297106614),
 .UNSPECIFIED.);
#190=B_SPLINE_CURVE_WITH_KNOTS('',3,(#7453,#7454,#7455,#7456,#7457,#7458,
#7459,#7460,#7461,#7462,#7463,#7464,#7465,#7466,#7467,#7468,#7469,#7470),
 .UNSPECIFIED.,.F.,.F.,(4,2,2,2,2,2,2,2,4),(0.313885742766535,0.391923143756543,
0.46996054474655,0.54886601513981,0.62777148553307,0.70667695592633,0.785582426319589,
0.863619827309597,0.941657228299605),.UNSPECIFIED.);
#191=B_SPLINE_CURVE_WITH_KNOTS('',3,(#7481,#7482,#7483,#7484,#7485,#7486,
#7487,#7488,#7489,#7490),.UNSPECIFIED.,.F.,.F.,(4,2,2,2,4),(0.,0.0789054703932594,
0.157810940786519,0.235848341776527,0.313885742766535),.UNSPECIFIED.);
#192=B_SPLINE_CURVE_WITH_KNOTS('',3,(#7492,#7493,#7494,#7495,#7496,#7497,
#7498,#7499,#7500,#7501),.UNSPECIFIED.,.F.,.F.,(4,2,2,2,4),(0.941657228299605,
1.01969462928961,1.09773203027962,1.17663750067288,1.25554297106614),
 .UNSPECIFIED.);
#193=B_SPLINE_CURVE_WITH_KNOTS('',3,(#7505,#7506,#7507,#7508,#7509,#7510,
#7511,#7512,#7513,#7514,#7515,#7516,#7517,#7518,#7519,#7520,#7521,#7522),
 .UNSPECIFIED.,.F.,.F.,(4,2,2,2,2,2,2,2,4),(0.313885742766535,0.391923143756543,
0.46996054474655,0.54886601513981,0.62777148553307,0.70667695592633,0.785582426319589,
0.863619827309597,0.941657228299605),.UNSPECIFIED.);
#194=B_SPLINE_CURVE_WITH_KNOTS('',3,(#7533,#7534,#7535,#7536,#7537,#7538,
#7539,#7540,#7541,#7542),.UNSPECIFIED.,.F.,.F.,(4,2,2,2,4),(0.,0.0789054703932596,
0.157810940786519,0.235848341776527,0.313885742766535),.UNSPECIFIED.);
#195=B_SPLINE_CURVE_WITH_KNOTS('',3,(#7544,#7545,#7546,#7547,#7548,#7549,
#7550,#7551,#7552,#7553),.UNSPECIFIED.,.F.,.F.,(4,2,2,2,4),(0.941657228299606,
1.01969462928961,1.09773203027962,1.17663750067288,1.25554297106614),
 .UNSPECIFIED.);
#196=B_SPLINE_CURVE_WITH_KNOTS('',3,(#7557,#7558,#7559,#7560,#7561,#7562,
#7563,#7564,#7565,#7566,#7567,#7568,#7569,#7570,#7571,#7572,#7573,#7574),
 .UNSPECIFIED.,.F.,.F.,(4,2,2,2,2,2,2,2,4),(0.313885742766535,0.391923143756543,
0.469960544746551,0.548866015139811,0.62777148553307,0.70667695592633,0.78558242631959,
0.863619827309598,0.941657228299606),.UNSPECIFIED.);
#197=SHAPE_REPRESENTATION_RELATIONSHIP('SRR','None',#8359,#219);
#198=SHAPE_REPRESENTATION_RELATIONSHIP('SRR','None',#8360,#220);
#199=SHAPE_REPRESENTATION_RELATIONSHIP('SRR','None',#8361,#221);
#200=SHAPE_REPRESENTATION_RELATIONSHIP('SRR','None',#8362,#222);
#201=SHAPE_REPRESENTATION_RELATIONSHIP('SRR','None',#8363,#223);
#202=SHAPE_REPRESENTATION_RELATIONSHIP('SRR','None',#8364,#224);
#203=SHAPE_REPRESENTATION_RELATIONSHIP('SRR','None',#8365,#225);
#204=SHAPE_REPRESENTATION_RELATIONSHIP('SRR','None',#8366,#226);
#205=SHAPE_REPRESENTATION_RELATIONSHIP('SRR','None',#8367,#227);
#206=SHAPE_REPRESENTATION_RELATIONSHIP('SRR','None',#8368,#228);
#207=SHAPE_REPRESENTATION_RELATIONSHIP('SRR','None',#8369,#229);
#208=SHAPE_REPRESENTATION_RELATIONSHIP('SRR','None',#8370,#230);
#209=SHAPE_REPRESENTATION_RELATIONSHIP('SRR','None',#8371,#231);
#210=SHAPE_REPRESENTATION_RELATIONSHIP('SRR','None',#8372,#232);
#211=SHAPE_REPRESENTATION_RELATIONSHIP('SRR','None',#8373,#233);
#212=SHAPE_REPRESENTATION_RELATIONSHIP('SRR','None',#8374,#234);
#213=SHAPE_REPRESENTATION_RELATIONSHIP('SRR','None',#8375,#235);
#214=SHAPE_REPRESENTATION_RELATIONSHIP('SRR','None',#8377,#236);
#215=SHAPE_REPRESENTATION_RELATIONSHIP('SRR','None',#8378,#237);
#216=SHAPE_REPRESENTATION_RELATIONSHIP('SRR','None',#8379,#238);
#217=SHAPE_REPRESENTATION_RELATIONSHIP('SRR','None',#8380,#239);
#218=SHAPE_REPRESENTATION_RELATIONSHIP('SRR','None',#8381,#240);
#219=ADVANCED_BREP_SHAPE_REPRESENTATION('',(#263),#8243);
#220=ADVANCED_BREP_SHAPE_REPRESENTATION('',(#264),#8244);
#221=ADVANCED_BREP_SHAPE_REPRESENTATION('',(#265),#8245);
#222=ADVANCED_BREP_SHAPE_REPRESENTATION('',(#266),#8246);
#223=ADVANCED_BREP_SHAPE_REPRESENTATION('',(#267),#8247);
#224=ADVANCED_BREP_SHAPE_REPRESENTATION('',(#268),#8248);
#225=ADVANCED_BREP_SHAPE_REPRESENTATION('',(#269),#8249);
#226=ADVANCED_BREP_SHAPE_REPRESENTATION('',(#270),#8250);
#227=ADVANCED_BREP_SHAPE_REPRESENTATION('',(#271),#8251);
#228=ADVANCED_BREP_SHAPE_REPRESENTATION('',(#272),#8252);
#229=ADVANCED_BREP_SHAPE_REPRESENTATION('',(#273),#8253);
#230=ADVANCED_BREP_SHAPE_REPRESENTATION('',(#274),#8254);
#231=ADVANCED_BREP_SHAPE_REPRESENTATION('',(#275),#8255);
#232=ADVANCED_BREP_SHAPE_REPRESENTATION('',(#276),#8256);
#233=ADVANCED_BREP_SHAPE_REPRESENTATION('',(#277),#8257);
#234=ADVANCED_BREP_SHAPE_REPRESENTATION('',(#278),#8258);
#235=ADVANCED_BREP_SHAPE_REPRESENTATION('',(#182),#8259);
#236=ADVANCED_BREP_SHAPE_REPRESENTATION('',(#279),#8261);
#237=ADVANCED_BREP_SHAPE_REPRESENTATION('',(#280),#8262);
#238=ADVANCED_BREP_SHAPE_REPRESENTATION('',(#281),#8263);
#239=ADVANCED_BREP_SHAPE_REPRESENTATION('',(#183),#8264);
#240=ADVANCED_BREP_SHAPE_REPRESENTATION('',(#184),#8265);
#241=STYLED_ITEM('',(#8516),#263);
#242=STYLED_ITEM('',(#8551),#264);
#243=STYLED_ITEM('',(#8551),#265);
#244=STYLED_ITEM('',(#8530),#266);
#245=STYLED_ITEM('',(#8530),#267);
#246=STYLED_ITEM('',(#8551),#268);
#247=STYLED_ITEM('',(#8530),#269);
#248=STYLED_ITEM('',(#8516),#270);
#249=STYLED_ITEM('',(#8530),#271);
#250=STYLED_ITEM('',(#8530),#272);
#251=STYLED_ITEM('',(#8530),#273);
#252=STYLED_ITEM('',(#8530),#274);
#253=STYLED_ITEM('',(#8551),#275);
#254=STYLED_ITEM('',(#8530),#276);
#255=STYLED_ITEM('',(#8530),#277);
#256=STYLED_ITEM('',(#8523),#278);
#257=STYLED_ITEM('',(#8544),#182);
#258=STYLED_ITEM('',(#8516),#279);
#259=STYLED_ITEM('',(#8551),#280);
#260=STYLED_ITEM('',(#8530),#281);
#261=STYLED_ITEM('',(#8544),#183);
#262=STYLED_ITEM('',(#8544),#184);
#263=MANIFOLD_SOLID_BREP('Body1',#4581);
#264=MANIFOLD_SOLID_BREP('Body1',#4582);
#265=MANIFOLD_SOLID_BREP('Body1',#4583);
#266=MANIFOLD_SOLID_BREP('Body1',#4584);
#267=MANIFOLD_SOLID_BREP('Body1',#4585);
#268=MANIFOLD_SOLID_BREP('Body1',#4586);
#269=MANIFOLD_SOLID_BREP('Body1',#4587);
#270=MANIFOLD_SOLID_BREP('Body1',#4588);
#271=MANIFOLD_SOLID_BREP('Body1',#4589);
#272=MANIFOLD_SOLID_BREP('Body1',#4590);
#273=MANIFOLD_SOLID_BREP('Body1',#4591);
#274=MANIFOLD_SOLID_BREP('Body1',#4592);
#275=MANIFOLD_SOLID_BREP('Body1',#4593);
#276=MANIFOLD_SOLID_BREP('Body1',#4594);
#277=MANIFOLD_SOLID_BREP('Body1',#4595);
#278=MANIFOLD_SOLID_BREP('Body1',#4596);
#279=MANIFOLD_SOLID_BREP('Body1',#4599);
#280=MANIFOLD_SOLID_BREP('Body1',#4600);
#281=MANIFOLD_SOLID_BREP('Body1',#4601);
#282=FACE_BOUND('',#859,.T.);
#283=FACE_BOUND('',#860,.T.);
#284=FACE_BOUND('',#861,.T.);
#285=FACE_BOUND('',#862,.T.);
#286=FACE_BOUND('',#863,.T.);
#287=FACE_BOUND('',#864,.T.);
#288=FACE_BOUND('',#865,.T.);
#289=FACE_BOUND('',#866,.T.);
#290=FACE_BOUND('',#868,.T.);
#291=FACE_BOUND('',#869,.T.);
#292=FACE_BOUND('',#870,.T.);
#293=FACE_BOUND('',#871,.T.);
#294=FACE_BOUND('',#897,.T.);
#295=FACE_BOUND('',#898,.T.);
#296=FACE_BOUND('',#899,.T.);
#297=FACE_BOUND('',#900,.T.);
#298=FACE_BOUND('',#902,.T.);
#299=FACE_BOUND('',#903,.T.);
#300=FACE_BOUND('',#904,.T.);
#301=FACE_BOUND('',#905,.T.);
#302=FACE_BOUND('',#919,.T.);
#303=FACE_BOUND('',#920,.T.);
#304=FACE_BOUND('',#921,.T.);
#305=FACE_BOUND('',#922,.T.);
#306=FACE_BOUND('',#924,.T.);
#307=FACE_BOUND('',#925,.T.);
#308=FACE_BOUND('',#926,.T.);
#309=FACE_BOUND('',#927,.T.);
#310=FACE_BOUND('',#945,.T.);
#311=FACE_BOUND('',#946,.T.);
#312=FACE_BOUND('',#947,.T.);
#313=FACE_BOUND('',#948,.T.);
#314=FACE_BOUND('',#949,.T.);
#315=FACE_BOUND('',#950,.T.);
#316=FACE_BOUND('',#951,.T.);
#317=FACE_BOUND('',#952,.T.);
#318=FACE_BOUND('',#953,.T.);
#319=FACE_BOUND('',#954,.T.);
#320=FACE_BOUND('',#955,.T.);
#321=FACE_BOUND('',#956,.T.);
#322=FACE_BOUND('',#958,.T.);
#323=FACE_BOUND('',#959,.T.);
#324=FACE_BOUND('',#960,.T.);
#325=FACE_BOUND('',#961,.T.);
#326=FACE_BOUND('',#962,.T.);
#327=FACE_BOUND('',#963,.T.);
#328=FACE_BOUND('',#964,.T.);
#329=FACE_BOUND('',#965,.T.);
#330=FACE_BOUND('',#966,.T.);
#331=FACE_BOUND('',#967,.T.);
#332=FACE_BOUND('',#968,.T.);
#333=FACE_BOUND('',#969,.T.);
#334=FACE_BOUND('',#987,.T.);
#335=FACE_BOUND('',#988,.T.);
#336=FACE_BOUND('',#989,.T.);
#337=FACE_BOUND('',#990,.T.);
#338=FACE_BOUND('',#991,.T.);
#339=FACE_BOUND('',#992,.T.);
#340=FACE_BOUND('',#993,.T.);
#341=FACE_BOUND('',#994,.T.);
#342=FACE_BOUND('',#995,.T.);
#343=FACE_BOUND('',#997,.T.);
#344=FACE_BOUND('',#998,.T.);
#345=FACE_BOUND('',#999,.T.);
#346=FACE_BOUND('',#1000,.T.);
#347=FACE_BOUND('',#1001,.T.);
#348=FACE_BOUND('',#1002,.T.);
#349=FACE_BOUND('',#1003,.T.);
#350=FACE_BOUND('',#1004,.T.);
#351=FACE_BOUND('',#1005,.T.);
#352=FACE_BOUND('',#1028,.T.);
#353=FACE_BOUND('',#1031,.T.);
#354=FACE_BOUND('',#1035,.T.);
#355=FACE_BOUND('',#1039,.T.);
#356=FACE_BOUND('',#1043,.T.);
#357=FACE_BOUND('',#1047,.T.);
#358=FACE_BOUND('',#1055,.T.);
#359=FACE_BOUND('',#1058,.T.);
#360=FACE_BOUND('',#1060,.T.);
#361=FACE_BOUND('',#1061,.T.);
#362=FACE_BOUND('',#1063,.T.);
#363=FACE_BOUND('',#1065,.T.);
#364=FACE_BOUND('',#1066,.T.);
#365=FACE_BOUND('',#1067,.T.);
#366=FACE_BOUND('',#1068,.T.);
#367=FACE_BOUND('',#1070,.T.);
#368=FACE_BOUND('',#1071,.T.);
#369=FACE_BOUND('',#1072,.T.);
#370=FACE_BOUND('',#1073,.T.);
#371=FACE_BOUND('',#1074,.T.);
#372=FACE_BOUND('',#1075,.T.);
#373=FACE_BOUND('',#1076,.T.);
#374=FACE_BOUND('',#1077,.T.);
#375=FACE_BOUND('',#1078,.T.);
#376=FACE_BOUND('',#1082,.T.);
#377=FACE_BOUND('',#1084,.T.);
#378=FACE_BOUND('',#1088,.T.);
#379=FACE_BOUND('',#1090,.T.);
#380=FACE_BOUND('',#1094,.T.);
#381=FACE_BOUND('',#1096,.T.);
#382=FACE_BOUND('',#1100,.T.);
#383=FACE_BOUND('',#1102,.T.);
#384=FACE_BOUND('',#1104,.T.);
#385=FACE_BOUND('',#1123,.T.);
#386=FACE_BOUND('',#1124,.T.);
#387=FACE_BOUND('',#1127,.T.);
#388=FACE_BOUND('',#1128,.T.);
#389=FACE_BOUND('',#1146,.T.);
#390=FACE_BOUND('',#1151,.T.);
#391=FACE_BOUND('',#1153,.T.);
#392=FACE_BOUND('',#1155,.T.);
#393=FACE_BOUND('',#1163,.T.);
#394=FACE_BOUND('',#1166,.T.);
#395=FACE_BOUND('',#1170,.T.);
#396=FACE_BOUND('',#1173,.T.);
#397=FACE_BOUND('',#1176,.T.);
#398=FACE_BOUND('',#1179,.T.);
#399=FACE_BOUND('',#1182,.T.);
#400=FACE_BOUND('',#1184,.T.);
#401=FACE_BOUND('',#1193,.T.);
#402=FACE_BOUND('',#1198,.T.);
#403=FACE_BOUND('',#1205,.T.);
#404=FACE_BOUND('',#1232,.T.);
#405=PLANE('',#4854);
#406=PLANE('',#4858);
#407=PLANE('',#4862);
#408=PLANE('',#4866);
#409=PLANE('',#4879);
#410=PLANE('',#4880);
#411=PLANE('',#4881);
#412=PLANE('',#4882);
#413=PLANE('',#4883);
#414=PLANE('',#4884);
#415=PLANE('',#4886);
#416=PLANE('',#4887);
#417=PLANE('',#4888);
#418=PLANE('',#4889);
#419=PLANE('',#4890);
#420=PLANE('',#4891);
#421=PLANE('',#4893);
#422=PLANE('',#4894);
#423=PLANE('',#4895);
#424=PLANE('',#4896);
#425=PLANE('',#4897);
#426=PLANE('',#4898);
#427=PLANE('',#4900);
#428=PLANE('',#4905);
#429=PLANE('',#4924);
#430=PLANE('',#4925);
#431=PLANE('',#4926);
#432=PLANE('',#4927);
#433=PLANE('',#4928);
#434=PLANE('',#4929);
#435=PLANE('',#4931);
#436=PLANE('',#4936);
#437=PLANE('',#4955);
#438=PLANE('',#4956);
#439=PLANE('',#4957);
#440=PLANE('',#4958);
#441=PLANE('',#4959);
#442=PLANE('',#4960);
#443=PLANE('',#4998);
#444=PLANE('',#4999);
#445=PLANE('',#5000);
#446=PLANE('',#5001);
#447=PLANE('',#5002);
#448=PLANE('',#5003);
#449=PLANE('',#5029);
#450=PLANE('',#5030);
#451=PLANE('',#5031);
#452=PLANE('',#5032);
#453=PLANE('',#5033);
#454=PLANE('',#5034);
#455=PLANE('',#5035);
#456=PLANE('',#5036);
#457=PLANE('',#5037);
#458=PLANE('',#5038);
#459=PLANE('',#5043);
#460=PLANE('',#5047);
#461=PLANE('',#5051);
#462=PLANE('',#5055);
#463=PLANE('',#5059);
#464=PLANE('',#5063);
#465=PLANE('',#5067);
#466=PLANE('',#5071);
#467=PLANE('',#5075);
#468=PLANE('',#5079);
#469=PLANE('',#5083);
#470=PLANE('',#5088);
#471=PLANE('',#5095);
#472=PLANE('',#5101);
#473=PLANE('',#5107);
#474=PLANE('',#5113);
#475=PLANE('',#5114);
#476=PLANE('',#5115);
#477=PLANE('',#5117);
#478=PLANE('',#5118);
#479=PLANE('',#5119);
#480=PLANE('',#5121);
#481=PLANE('',#5123);
#482=PLANE('',#5124);
#483=PLANE('',#5125);
#484=PLANE('',#5126);
#485=PLANE('',#5127);
#486=PLANE('',#5128);
#487=PLANE('',#5136);
#488=PLANE('',#5137);
#489=PLANE('',#5145);
#490=PLANE('',#5146);
#491=PLANE('',#5154);
#492=PLANE('',#5155);
#493=PLANE('',#5163);
#494=PLANE('',#5164);
#495=PLANE('',#5166);
#496=PLANE('',#5168);
#497=PLANE('',#5169);
#498=PLANE('',#5170);
#499=PLANE('',#5171);
#500=PLANE('',#5172);
#501=PLANE('',#5173);
#502=PLANE('',#5174);
#503=PLANE('',#5177);
#504=PLANE('',#5182);
#505=PLANE('',#5183);
#506=PLANE('',#5188);
#507=PLANE('',#5189);
#508=PLANE('',#5197);
#509=PLANE('',#5198);
#510=PLANE('',#5199);
#511=PLANE('',#5200);
#512=PLANE('',#5201);
#513=PLANE('',#5202);
#514=PLANE('',#5204);
#515=PLANE('',#5205);
#516=PLANE('',#5206);
#517=PLANE('',#5207);
#518=PLANE('',#5208);
#519=PLANE('',#5209);
#520=PLANE('',#5210);
#521=PLANE('',#5211);
#522=PLANE('',#5212);
#523=PLANE('',#5214);
#524=PLANE('',#5222);
#525=PLANE('',#5232);
#526=PLANE('',#5234);
#527=PLANE('',#5236);
#528=PLANE('',#5238);
#529=PLANE('',#5239);
#530=PLANE('',#5240);
#531=PLANE('',#5241);
#532=PLANE('',#5242);
#533=PLANE('',#5243);
#534=PLANE('',#5244);
#535=PLANE('',#5248);
#536=PLANE('',#5253);
#537=PLANE('',#5257);
#538=PLANE('',#5262);
#539=PLANE('',#5266);
#540=PLANE('',#5272);
#541=PLANE('',#5274);
#542=PLANE('',#5276);
#543=PLANE('',#5277);
#544=PLANE('',#5278);
#545=PLANE('',#5279);
#546=PLANE('',#5280);
#547=PLANE('',#5281);
#548=PLANE('',#5284);
#549=PLANE('',#5292);
#550=PLANE('',#5296);
#551=PLANE('',#5304);
#552=PLANE('',#5312);
#553=PLANE('',#5313);
#554=PLANE('',#5314);
#555=PLANE('',#5315);
#556=PLANE('',#5316);
#557=PLANE('',#5317);
#558=PLANE('',#5318);
#559=PLANE('',#5319);
#560=PLANE('',#5320);
#561=PLANE('',#5322);
#562=PLANE('',#5323);
#563=PLANE('',#5324);
#564=PLANE('',#5325);
#565=PLANE('',#5326);
#566=PLANE('',#5327);
#567=PLANE('',#5328);
#568=PLANE('',#5329);
#569=PLANE('',#5330);
#570=PLANE('',#5332);
#571=PLANE('',#5340);
#572=FACE_OUTER_BOUND('',#842,.T.);
#573=FACE_OUTER_BOUND('',#843,.T.);
#574=FACE_OUTER_BOUND('',#844,.T.);
#575=FACE_OUTER_BOUND('',#845,.T.);
#576=FACE_OUTER_BOUND('',#846,.T.);
#577=FACE_OUTER_BOUND('',#847,.T.);
#578=FACE_OUTER_BOUND('',#848,.T.);
#579=FACE_OUTER_BOUND('',#849,.T.);
#580=FACE_OUTER_BOUND('',#850,.T.);
#581=FACE_OUTER_BOUND('',#851,.T.);
#582=FACE_OUTER_BOUND('',#852,.T.);
#583=FACE_OUTER_BOUND('',#853,.T.);
#584=FACE_OUTER_BOUND('',#854,.T.);
#585=FACE_OUTER_BOUND('',#855,.T.);
#586=FACE_OUTER_BOUND('',#856,.T.);
#587=FACE_OUTER_BOUND('',#857,.T.);
#588=FACE_OUTER_BOUND('',#858,.T.);
#589=FACE_OUTER_BOUND('',#867,.T.);
#590=FACE_OUTER_BOUND('',#872,.T.);
#591=FACE_OUTER_BOUND('',#873,.T.);
#592=FACE_OUTER_BOUND('',#874,.T.);
#593=FACE_OUTER_BOUND('',#875,.T.);
#594=FACE_OUTER_BOUND('',#876,.T.);
#595=FACE_OUTER_BOUND('',#877,.T.);
#596=FACE_OUTER_BOUND('',#878,.T.);
#597=FACE_OUTER_BOUND('',#879,.T.);
#598=FACE_OUTER_BOUND('',#880,.T.);
#599=FACE_OUTER_BOUND('',#881,.T.);
#600=FACE_OUTER_BOUND('',#882,.T.);
#601=FACE_OUTER_BOUND('',#883,.T.);
#602=FACE_OUTER_BOUND('',#884,.T.);
#603=FACE_OUTER_BOUND('',#885,.T.);
#604=FACE_OUTER_BOUND('',#886,.T.);
#605=FACE_OUTER_BOUND('',#887,.T.);
#606=FACE_OUTER_BOUND('',#888,.T.);
#607=FACE_OUTER_BOUND('',#889,.T.);
#608=FACE_OUTER_BOUND('',#890,.T.);
#609=FACE_OUTER_BOUND('',#891,.T.);
#610=FACE_OUTER_BOUND('',#892,.T.);
#611=FACE_OUTER_BOUND('',#893,.T.);
#612=FACE_OUTER_BOUND('',#894,.T.);
#613=FACE_OUTER_BOUND('',#895,.T.);
#614=FACE_OUTER_BOUND('',#896,.T.);
#615=FACE_OUTER_BOUND('',#901,.T.);
#616=FACE_OUTER_BOUND('',#906,.T.);
#617=FACE_OUTER_BOUND('',#907,.T.);
#618=FACE_OUTER_BOUND('',#908,.T.);
#619=FACE_OUTER_BOUND('',#909,.T.);
#620=FACE_OUTER_BOUND('',#910,.T.);
#621=FACE_OUTER_BOUND('',#911,.T.);
#622=FACE_OUTER_BOUND('',#912,.T.);
#623=FACE_OUTER_BOUND('',#913,.T.);
#624=FACE_OUTER_BOUND('',#914,.T.);
#625=FACE_OUTER_BOUND('',#915,.T.);
#626=FACE_OUTER_BOUND('',#916,.T.);
#627=FACE_OUTER_BOUND('',#917,.T.);
#628=FACE_OUTER_BOUND('',#918,.T.);
#629=FACE_OUTER_BOUND('',#923,.T.);
#630=FACE_OUTER_BOUND('',#928,.T.);
#631=FACE_OUTER_BOUND('',#929,.T.);
#632=FACE_OUTER_BOUND('',#930,.T.);
#633=FACE_OUTER_BOUND('',#931,.T.);
#634=FACE_OUTER_BOUND('',#932,.T.);
#635=FACE_OUTER_BOUND('',#933,.T.);
#636=FACE_OUTER_BOUND('',#934,.T.);
#637=FACE_OUTER_BOUND('',#935,.T.);
#638=FACE_OUTER_BOUND('',#936,.T.);
#639=FACE_OUTER_BOUND('',#937,.T.);
#640=FACE_OUTER_BOUND('',#938,.T.);
#641=FACE_OUTER_BOUND('',#939,.T.);
#642=FACE_OUTER_BOUND('',#940,.T.);
#643=FACE_OUTER_BOUND('',#941,.T.);
#644=FACE_OUTER_BOUND('',#942,.T.);
#645=FACE_OUTER_BOUND('',#943,.T.);
#646=FACE_OUTER_BOUND('',#944,.T.);
#647=FACE_OUTER_BOUND('',#957,.T.);
#648=FACE_OUTER_BOUND('',#970,.T.);
#649=FACE_OUTER_BOUND('',#971,.T.);
#650=FACE_OUTER_BOUND('',#972,.T.);
#651=FACE_OUTER_BOUND('',#973,.T.);
#652=FACE_OUTER_BOUND('',#974,.T.);
#653=FACE_OUTER_BOUND('',#975,.T.);
#654=FACE_OUTER_BOUND('',#976,.T.);
#655=FACE_OUTER_BOUND('',#977,.T.);
#656=FACE_OUTER_BOUND('',#978,.T.);
#657=FACE_OUTER_BOUND('',#979,.T.);
#658=FACE_OUTER_BOUND('',#980,.T.);
#659=FACE_OUTER_BOUND('',#981,.T.);
#660=FACE_OUTER_BOUND('',#982,.T.);
#661=FACE_OUTER_BOUND('',#983,.T.);
#662=FACE_OUTER_BOUND('',#984,.T.);
#663=FACE_OUTER_BOUND('',#985,.T.);
#664=FACE_OUTER_BOUND('',#986,.T.);
#665=FACE_OUTER_BOUND('',#996,.T.);
#666=FACE_OUTER_BOUND('',#1006,.T.);
#667=FACE_OUTER_BOUND('',#1007,.T.);
#668=FACE_OUTER_BOUND('',#1008,.T.);
#669=FACE_OUTER_BOUND('',#1009,.T.);
#670=FACE_OUTER_BOUND('',#1010,.T.);
#671=FACE_OUTER_BOUND('',#1011,.T.);
#672=FACE_OUTER_BOUND('',#1012,.T.);
#673=FACE_OUTER_BOUND('',#1013,.T.);
#674=FACE_OUTER_BOUND('',#1014,.T.);
#675=FACE_OUTER_BOUND('',#1015,.T.);
#676=FACE_OUTER_BOUND('',#1016,.T.);
#677=FACE_OUTER_BOUND('',#1017,.T.);
#678=FACE_OUTER_BOUND('',#1018,.T.);
#679=FACE_OUTER_BOUND('',#1019,.T.);
#680=FACE_OUTER_BOUND('',#1020,.T.);
#681=FACE_OUTER_BOUND('',#1021,.T.);
#682=FACE_OUTER_BOUND('',#1022,.T.);
#683=FACE_OUTER_BOUND('',#1023,.T.);
#684=FACE_OUTER_BOUND('',#1024,.T.);
#685=FACE_OUTER_BOUND('',#1025,.T.);
#686=FACE_OUTER_BOUND('',#1026,.T.);
#687=FACE_OUTER_BOUND('',#1027,.T.);
#688=FACE_OUTER_BOUND('',#1029,.T.);
#689=FACE_OUTER_BOUND('',#1030,.T.);
#690=FACE_OUTER_BOUND('',#1032,.T.);
#691=FACE_OUTER_BOUND('',#1033,.T.);
#692=FACE_OUTER_BOUND('',#1034,.T.);
#693=FACE_OUTER_BOUND('',#1036,.T.);
#694=FACE_OUTER_BOUND('',#1037,.T.);
#695=FACE_OUTER_BOUND('',#1038,.T.);
#696=FACE_OUTER_BOUND('',#1040,.T.);
#697=FACE_OUTER_BOUND('',#1041,.T.);
#698=FACE_OUTER_BOUND('',#1042,.T.);
#699=FACE_OUTER_BOUND('',#1044,.T.);
#700=FACE_OUTER_BOUND('',#1045,.T.);
#701=FACE_OUTER_BOUND('',#1046,.T.);
#702=FACE_OUTER_BOUND('',#1048,.T.);
#703=FACE_OUTER_BOUND('',#1049,.T.);
#704=FACE_OUTER_BOUND('',#1050,.T.);
#705=FACE_OUTER_BOUND('',#1051,.T.);
#706=FACE_OUTER_BOUND('',#1052,.T.);
#707=FACE_OUTER_BOUND('',#1053,.T.);
#708=FACE_OUTER_BOUND('',#1054,.T.);
#709=FACE_OUTER_BOUND('',#1056,.T.);
#710=FACE_OUTER_BOUND('',#1057,.T.);
#711=FACE_OUTER_BOUND('',#1059,.T.);
#712=FACE_OUTER_BOUND('',#1062,.T.);
#713=FACE_OUTER_BOUND('',#1064,.T.);
#714=FACE_OUTER_BOUND('',#1069,.T.);
#715=FACE_OUTER_BOUND('',#1079,.T.);
#716=FACE_OUTER_BOUND('',#1080,.T.);
#717=FACE_OUTER_BOUND('',#1081,.T.);
#718=FACE_OUTER_BOUND('',#1083,.T.);
#719=FACE_OUTER_BOUND('',#1085,.T.);
#720=FACE_OUTER_BOUND('',#1086,.T.);
#721=FACE_OUTER_BOUND('',#1087,.T.);
#722=FACE_OUTER_BOUND('',#1089,.T.);
#723=FACE_OUTER_BOUND('',#1091,.T.);
#724=FACE_OUTER_BOUND('',#1092,.T.);
#725=FACE_OUTER_BOUND('',#1093,.T.);
#726=FACE_OUTER_BOUND('',#1095,.T.);
#727=FACE_OUTER_BOUND('',#1097,.T.);
#728=FACE_OUTER_BOUND('',#1098,.T.);
#729=FACE_OUTER_BOUND('',#1099,.T.);
#730=FACE_OUTER_BOUND('',#1101,.T.);
#731=FACE_OUTER_BOUND('',#1103,.T.);
#732=FACE_OUTER_BOUND('',#1105,.T.);
#733=FACE_OUTER_BOUND('',#1106,.T.);
#734=FACE_OUTER_BOUND('',#1107,.T.);
#735=FACE_OUTER_BOUND('',#1108,.T.);
#736=FACE_OUTER_BOUND('',#1109,.T.);
#737=FACE_OUTER_BOUND('',#1110,.T.);
#738=FACE_OUTER_BOUND('',#1111,.T.);
#739=FACE_OUTER_BOUND('',#1112,.T.);
#740=FACE_OUTER_BOUND('',#1113,.T.);
#741=FACE_OUTER_BOUND('',#1114,.T.);
#742=FACE_OUTER_BOUND('',#1115,.T.);
#743=FACE_OUTER_BOUND('',#1116,.T.);
#744=FACE_OUTER_BOUND('',#1117,.T.);
#745=FACE_OUTER_BOUND('',#1118,.T.);
#746=FACE_OUTER_BOUND('',#1119,.T.);
#747=FACE_OUTER_BOUND('',#1120,.T.);
#748=FACE_OUTER_BOUND('',#1121,.T.);
#749=FACE_OUTER_BOUND('',#1122,.T.);
#750=FACE_OUTER_BOUND('',#1125,.T.);
#751=FACE_OUTER_BOUND('',#1126,.T.);
#752=FACE_OUTER_BOUND('',#1129,.T.);
#753=FACE_OUTER_BOUND('',#1130,.T.);
#754=FACE_OUTER_BOUND('',#1131,.T.);
#755=FACE_OUTER_BOUND('',#1132,.T.);
#756=FACE_OUTER_BOUND('',#1133,.T.);
#757=FACE_OUTER_BOUND('',#1134,.T.);
#758=FACE_OUTER_BOUND('',#1135,.T.);
#759=FACE_OUTER_BOUND('',#1136,.T.);
#760=FACE_OUTER_BOUND('',#1137,.T.);
#761=FACE_OUTER_BOUND('',#1138,.T.);
#762=FACE_OUTER_BOUND('',#1139,.T.);
#763=FACE_OUTER_BOUND('',#1140,.T.);
#764=FACE_OUTER_BOUND('',#1141,.T.);
#765=FACE_OUTER_BOUND('',#1142,.T.);
#766=FACE_OUTER_BOUND('',#1143,.T.);
#767=FACE_OUTER_BOUND('',#1144,.T.);
#768=FACE_OUTER_BOUND('',#1145,.T.);
#769=FACE_OUTER_BOUND('',#1147,.T.);
#770=FACE_OUTER_BOUND('',#1148,.T.);
#771=FACE_OUTER_BOUND('',#1149,.T.);
#772=FACE_OUTER_BOUND('',#1150,.T.);
#773=FACE_OUTER_BOUND('',#1152,.T.);
#774=FACE_OUTER_BOUND('',#1154,.T.);
#775=FACE_OUTER_BOUND('',#1156,.T.);
#776=FACE_OUTER_BOUND('',#1157,.T.);
#777=FACE_OUTER_BOUND('',#1158,.T.);
#778=FACE_OUTER_BOUND('',#1159,.T.);
#779=FACE_OUTER_BOUND('',#1160,.T.);
#780=FACE_OUTER_BOUND('',#1161,.T.);
#781=FACE_OUTER_BOUND('',#1162,.T.);
#782=FACE_OUTER_BOUND('',#1164,.T.);
#783=FACE_OUTER_BOUND('',#1165,.T.);
#784=FACE_OUTER_BOUND('',#1167,.T.);
#785=FACE_OUTER_BOUND('',#1168,.T.);
#786=FACE_OUTER_BOUND('',#1169,.T.);
#787=FACE_OUTER_BOUND('',#1171,.T.);
#788=FACE_OUTER_BOUND('',#1172,.T.);
#789=FACE_OUTER_BOUND('',#1174,.T.);
#790=FACE_OUTER_BOUND('',#1175,.T.);
#791=FACE_OUTER_BOUND('',#1177,.T.);
#792=FACE_OUTER_BOUND('',#1178,.T.);
#793=FACE_OUTER_BOUND('',#1180,.T.);
#794=FACE_OUTER_BOUND('',#1181,.T.);
#795=FACE_OUTER_BOUND('',#1183,.T.);
#796=FACE_OUTER_BOUND('',#1185,.T.);
#797=FACE_OUTER_BOUND('',#1186,.T.);
#798=FACE_OUTER_BOUND('',#1187,.T.);
#799=FACE_OUTER_BOUND('',#1188,.T.);
#800=FACE_OUTER_BOUND('',#1189,.T.);
#801=FACE_OUTER_BOUND('',#1190,.T.);
#802=FACE_OUTER_BOUND('',#1191,.T.);
#803=FACE_OUTER_BOUND('',#1192,.T.);
#804=FACE_OUTER_BOUND('',#1194,.T.);
#805=FACE_OUTER_BOUND('',#1195,.T.);
#806=FACE_OUTER_BOUND('',#1196,.T.);
#807=FACE_OUTER_BOUND('',#1197,.T.);
#808=FACE_OUTER_BOUND('',#1199,.T.);
#809=FACE_OUTER_BOUND('',#1200,.T.);
#810=FACE_OUTER_BOUND('',#1201,.T.);
#811=FACE_OUTER_BOUND('',#1202,.T.);
#812=FACE_OUTER_BOUND('',#1203,.T.);
#813=FACE_OUTER_BOUND('',#1204,.T.);
#814=FACE_OUTER_BOUND('',#1206,.T.);
#815=FACE_OUTER_BOUND('',#1207,.T.);
#816=FACE_OUTER_BOUND('',#1208,.T.);
#817=FACE_OUTER_BOUND('',#1209,.T.);
#818=FACE_OUTER_BOUND('',#1210,.T.);
#819=FACE_OUTER_BOUND('',#1211,.T.);
#820=FACE_OUTER_BOUND('',#1212,.T.);
#821=FACE_OUTER_BOUND('',#1213,.T.);
#822=FACE_OUTER_BOUND('',#1214,.T.);
#823=FACE_OUTER_BOUND('',#1215,.T.);
#824=FACE_OUTER_BOUND('',#1216,.T.);
#825=FACE_OUTER_BOUND('',#1217,.T.);
#826=FACE_OUTER_BOUND('',#1218,.T.);
#827=FACE_OUTER_BOUND('',#1219,.T.);
#828=FACE_OUTER_BOUND('',#1220,.T.);
#829=FACE_OUTER_BOUND('',#1221,.T.);
#830=FACE_OUTER_BOUND('',#1222,.T.);
#831=FACE_OUTER_BOUND('',#1223,.T.);
#832=FACE_OUTER_BOUND('',#1224,.T.);
#833=FACE_OUTER_BOUND('',#1225,.T.);
#834=FACE_OUTER_BOUND('',#1226,.T.);
#835=FACE_OUTER_BOUND('',#1227,.T.);
#836=FACE_OUTER_BOUND('',#1228,.T.);
#837=FACE_OUTER_BOUND('',#1229,.T.);
#838=FACE_OUTER_BOUND('',#1230,.T.);
#839=FACE_OUTER_BOUND('',#1231,.T.);
#840=FACE_OUTER_BOUND('',#1233,.T.);
#841=FACE_OUTER_BOUND('',#1234,.T.);
#842=EDGE_LOOP('',(#3086,#3087,#3088,#3089));
#843=EDGE_LOOP('',(#3090));
#844=EDGE_LOOP('',(#3091,#3092,#3093,#3094));
#845=EDGE_LOOP('',(#3095));
#846=EDGE_LOOP('',(#3096,#3097,#3098,#3099));
#847=EDGE_LOOP('',(#3100));
#848=EDGE_LOOP('',(#3101,#3102,#3103,#3104));
#849=EDGE_LOOP('',(#3105));
#850=EDGE_LOOP('',(#3106,#3107,#3108,#3109));
#851=EDGE_LOOP('',(#3110,#3111,#3112,#3113));
#852=EDGE_LOOP('',(#3114,#3115,#3116,#3117));
#853=EDGE_LOOP('',(#3118,#3119,#3120,#3121));
#854=EDGE_LOOP('',(#3122,#3123,#3124,#3125));
#855=EDGE_LOOP('',(#3126,#3127,#3128,#3129));
#856=EDGE_LOOP('',(#3130,#3131,#3132,#3133));
#857=EDGE_LOOP('',(#3134,#3135,#3136,#3137));
#858=EDGE_LOOP('',(#3138,#3139,#3140,#3141));
#859=EDGE_LOOP('',(#3142));
#860=EDGE_LOOP('',(#3143));
#861=EDGE_LOOP('',(#3144));
#862=EDGE_LOOP('',(#3145));
#863=EDGE_LOOP('',(#3146));
#864=EDGE_LOOP('',(#3147));
#865=EDGE_LOOP('',(#3148));
#866=EDGE_LOOP('',(#3149));
#867=EDGE_LOOP('',(#3150,#3151,#3152,#3153));
#868=EDGE_LOOP('',(#3154));
#869=EDGE_LOOP('',(#3155));
#870=EDGE_LOOP('',(#3156));
#871=EDGE_LOOP('',(#3157));
#872=EDGE_LOOP('',(#3158,#3159,#3160,#3161));
#873=EDGE_LOOP('',(#3162,#3163,#3164,#3165));
#874=EDGE_LOOP('',(#3166,#3167,#3168,#3169));
#875=EDGE_LOOP('',(#3170,#3171,#3172,#3173));
#876=EDGE_LOOP('',(#3174,#3175,#3176,#3177));
#877=EDGE_LOOP('',(#3178,#3179,#3180,#3181));
#878=EDGE_LOOP('',(#3182,#3183,#3184,#3185));
#879=EDGE_LOOP('',(#3186,#3187,#3188,#3189));
#880=EDGE_LOOP('',(#3190,#3191,#3192,#3193));
#881=EDGE_LOOP('',(#3194,#3195,#3196,#3197));
#882=EDGE_LOOP('',(#3198,#3199,#3200,#3201));
#883=EDGE_LOOP('',(#3202,#3203,#3204,#3205));
#884=EDGE_LOOP('',(#3206,#3207));
#885=EDGE_LOOP('',(#3208,#3209,#3210,#3211));
#886=EDGE_LOOP('',(#3212,#3213));
#887=EDGE_LOOP('',(#3214,#3215,#3216,#3217));
#888=EDGE_LOOP('',(#3218,#3219,#3220,#3221,#3222,#3223,#3224,#3225));
#889=EDGE_LOOP('',(#3226,#3227,#3228,#3229,#3230,#3231,#3232,#3233));
#890=EDGE_LOOP('',(#3234,#3235,#3236,#3237));
#891=EDGE_LOOP('',(#3238,#3239,#3240,#3241));
#892=EDGE_LOOP('',(#3242,#3243,#3244,#3245));
#893=EDGE_LOOP('',(#3246,#3247,#3248,#3249));
#894=EDGE_LOOP('',(#3250,#3251,#3252,#3253));
#895=EDGE_LOOP('',(#3254,#3255,#3256,#3257));
#896=EDGE_LOOP('',(#3258,#3259,#3260,#3261));
#897=EDGE_LOOP('',(#3262,#3263,#3264));
#898=EDGE_LOOP('',(#3265,#3266,#3267));
#899=EDGE_LOOP('',(#3268));
#900=EDGE_LOOP('',(#3269));
#901=EDGE_LOOP('',(#3270,#3271,#3272,#3273));
#902=EDGE_LOOP('',(#3274));
#903=EDGE_LOOP('',(#3275));
#904=EDGE_LOOP('',(#3276));
#905=EDGE_LOOP('',(#3277));
#906=EDGE_LOOP('',(#3278,#3279));
#907=EDGE_LOOP('',(#3280,#3281,#3282,#3283));
#908=EDGE_LOOP('',(#3284,#3285));
#909=EDGE_LOOP('',(#3286,#3287,#3288,#3289));
#910=EDGE_LOOP('',(#3290,#3291,#3292,#3293,#3294,#3295,#3296,#3297));
#911=EDGE_LOOP('',(#3298,#3299,#3300,#3301,#3302,#3303,#3304,#3305));
#912=EDGE_LOOP('',(#3306,#3307,#3308,#3309));
#913=EDGE_LOOP('',(#3310,#3311,#3312,#3313));
#914=EDGE_LOOP('',(#3314,#3315,#3316,#3317));
#915=EDGE_LOOP('',(#3318,#3319,#3320,#3321));
#916=EDGE_LOOP('',(#3322,#3323,#3324,#3325));
#917=EDGE_LOOP('',(#3326,#3327,#3328,#3329));
#918=EDGE_LOOP('',(#3330,#3331,#3332,#3333));
#919=EDGE_LOOP('',(#3334,#3335,#3336));
#920=EDGE_LOOP('',(#3337,#3338,#3339));
#921=EDGE_LOOP('',(#3340));
#922=EDGE_LOOP('',(#3341));
#923=EDGE_LOOP('',(#3342,#3343,#3344,#3345));
#924=EDGE_LOOP('',(#3346));
#925=EDGE_LOOP('',(#3347));
#926=EDGE_LOOP('',(#3348));
#927=EDGE_LOOP('',(#3349));
#928=EDGE_LOOP('',(#3350,#3351,#3352,#3353));
#929=EDGE_LOOP('',(#3354,#3355,#3356,#3357));
#930=EDGE_LOOP('',(#3358,#3359,#3360,#3361));
#931=EDGE_LOOP('',(#3362,#3363,#3364,#3365));
#932=EDGE_LOOP('',(#3366,#3367,#3368,#3369));
#933=EDGE_LOOP('',(#3370,#3371,#3372,#3373));
#934=EDGE_LOOP('',(#3374,#3375,#3376,#3377));
#935=EDGE_LOOP('',(#3378,#3379,#3380,#3381));
#936=EDGE_LOOP('',(#3382,#3383,#3384,#3385));
#937=EDGE_LOOP('',(#3386,#3387,#3388,#3389));
#938=EDGE_LOOP('',(#3390,#3391,#3392,#3393));
#939=EDGE_LOOP('',(#3394,#3395,#3396,#3397));
#940=EDGE_LOOP('',(#3398,#3399,#3400,#3401));
#941=EDGE_LOOP('',(#3402,#3403,#3404,#3405));
#942=EDGE_LOOP('',(#3406,#3407,#3408,#3409));
#943=EDGE_LOOP('',(#3410,#3411,#3412,#3413));
#944=EDGE_LOOP('',(#3414,#3415,#3416,#3417));
#945=EDGE_LOOP('',(#3418));
#946=EDGE_LOOP('',(#3419));
#947=EDGE_LOOP('',(#3420));
#948=EDGE_LOOP('',(#3421));
#949=EDGE_LOOP('',(#3422));
#950=EDGE_LOOP('',(#3423));
#951=EDGE_LOOP('',(#3424));
#952=EDGE_LOOP('',(#3425));
#953=EDGE_LOOP('',(#3426));
#954=EDGE_LOOP('',(#3427));
#955=EDGE_LOOP('',(#3428));
#956=EDGE_LOOP('',(#3429));
#957=EDGE_LOOP('',(#3430,#3431,#3432,#3433));
#958=EDGE_LOOP('',(#3434));
#959=EDGE_LOOP('',(#3435));
#960=EDGE_LOOP('',(#3436));
#961=EDGE_LOOP('',(#3437));
#962=EDGE_LOOP('',(#3438));
#963=EDGE_LOOP('',(#3439));
#964=EDGE_LOOP('',(#3440));
#965=EDGE_LOOP('',(#3441));
#966=EDGE_LOOP('',(#3442));
#967=EDGE_LOOP('',(#3443));
#968=EDGE_LOOP('',(#3444));
#969=EDGE_LOOP('',(#3445));
#970=EDGE_LOOP('',(#3446,#3447,#3448,#3449));
#971=EDGE_LOOP('',(#3450,#3451,#3452,#3453));
#972=EDGE_LOOP('',(#3454,#3455,#3456,#3457));
#973=EDGE_LOOP('',(#3458,#3459,#3460,#3461));
#974=EDGE_LOOP('',(#3462,#3463,#3464,#3465));
#975=EDGE_LOOP('',(#3466,#3467,#3468,#3469));
#976=EDGE_LOOP('',(#3470,#3471,#3472,#3473));
#977=EDGE_LOOP('',(#3474,#3475,#3476,#3477));
#978=EDGE_LOOP('',(#3478,#3479,#3480,#3481));
#979=EDGE_LOOP('',(#3482,#3483,#3484,#3485));
#980=EDGE_LOOP('',(#3486,#3487,#3488,#3489));
#981=EDGE_LOOP('',(#3490,#3491,#3492,#3493));
#982=EDGE_LOOP('',(#3494,#3495,#3496,#3497));
#983=EDGE_LOOP('',(#3498,#3499,#3500,#3501));
#984=EDGE_LOOP('',(#3502,#3503,#3504,#3505));
#985=EDGE_LOOP('',(#3506,#3507,#3508,#3509));
#986=EDGE_LOOP('',(#3510,#3511,#3512,#3513));
#987=EDGE_LOOP('',(#3514));
#988=EDGE_LOOP('',(#3515,#3516,#3517,#3518));
#989=EDGE_LOOP('',(#3519));
#990=EDGE_LOOP('',(#3520));
#991=EDGE_LOOP('',(#3521));
#992=EDGE_LOOP('',(#3522));
#993=EDGE_LOOP('',(#3523));
#994=EDGE_LOOP('',(#3524));
#995=EDGE_LOOP('',(#3525));
#996=EDGE_LOOP('',(#3526,#3527,#3528,#3529));
#997=EDGE_LOOP('',(#3530));
#998=EDGE_LOOP('',(#3531,#3532,#3533,#3534));
#999=EDGE_LOOP('',(#3535));
#1000=EDGE_LOOP('',(#3536));
#1001=EDGE_LOOP('',(#3537));
#1002=EDGE_LOOP('',(#3538));
#1003=EDGE_LOOP('',(#3539));
#1004=EDGE_LOOP('',(#3540));
#1005=EDGE_LOOP('',(#3541));
#1006=EDGE_LOOP('',(#3542,#3543,#3544,#3545));
#1007=EDGE_LOOP('',(#3546));
#1008=EDGE_LOOP('',(#3547,#3548,#3549,#3550));
#1009=EDGE_LOOP('',(#3551));
#1010=EDGE_LOOP('',(#3552,#3553,#3554,#3555));
#1011=EDGE_LOOP('',(#3556));
#1012=EDGE_LOOP('',(#3557,#3558,#3559,#3560));
#1013=EDGE_LOOP('',(#3561));
#1014=EDGE_LOOP('',(#3562,#3563,#3564,#3565));
#1015=EDGE_LOOP('',(#3566));
#1016=EDGE_LOOP('',(#3567,#3568,#3569,#3570));
#1017=EDGE_LOOP('',(#3571));
#1018=EDGE_LOOP('',(#3572,#3573,#3574,#3575));
#1019=EDGE_LOOP('',(#3576));
#1020=EDGE_LOOP('',(#3577,#3578,#3579,#3580));
#1021=EDGE_LOOP('',(#3581));
#1022=EDGE_LOOP('',(#3582,#3583,#3584,#3585));
#1023=EDGE_LOOP('',(#3586));
#1024=EDGE_LOOP('',(#3587,#3588,#3589,#3590));
#1025=EDGE_LOOP('',(#3591));
#1026=EDGE_LOOP('',(#3592,#3593,#3594,#3595));
#1027=EDGE_LOOP('',(#3596));
#1028=EDGE_LOOP('',(#3597));
#1029=EDGE_LOOP('',(#3598,#3599,#3600,#3601));
#1030=EDGE_LOOP('',(#3602));
#1031=EDGE_LOOP('',(#3603));
#1032=EDGE_LOOP('',(#3604,#3605,#3606,#3607,#3608,#3609));
#1033=EDGE_LOOP('',(#3610,#3611,#3612,#3613));
#1034=EDGE_LOOP('',(#3614));
#1035=EDGE_LOOP('',(#3615));
#1036=EDGE_LOOP('',(#3616,#3617,#3618,#3619,#3620,#3621));
#1037=EDGE_LOOP('',(#3622,#3623,#3624,#3625));
#1038=EDGE_LOOP('',(#3626));
#1039=EDGE_LOOP('',(#3627));
#1040=EDGE_LOOP('',(#3628,#3629,#3630,#3631,#3632,#3633));
#1041=EDGE_LOOP('',(#3634,#3635,#3636,#3637));
#1042=EDGE_LOOP('',(#3638));
#1043=EDGE_LOOP('',(#3639));
#1044=EDGE_LOOP('',(#3640,#3641,#3642,#3643,#3644,#3645));
#1045=EDGE_LOOP('',(#3646,#3647,#3648,#3649));
#1046=EDGE_LOOP('',(#3650));
#1047=EDGE_LOOP('',(#3651));
#1048=EDGE_LOOP('',(#3652,#3653,#3654,#3655));
#1049=EDGE_LOOP('',(#3656,#3657,#3658,#3659,#3660,#3661));
#1050=EDGE_LOOP('',(#3662,#3663,#3664,#3665));
#1051=EDGE_LOOP('',(#3666,#3667,#3668,#3669));
#1052=EDGE_LOOP('',(#3670,#3671,#3672,#3673,#3674,#3675));
#1053=EDGE_LOOP('',(#3676,#3677,#3678,#3679));
#1054=EDGE_LOOP('',(#3680,#3681,#3682,#3683,#3684,#3685,#3686,#3687,#3688,
#3689,#3690,#3691,#3692,#3693,#3694,#3695,#3696,#3697,#3698,#3699,#3700,
#3701,#3702,#3703));
#1055=EDGE_LOOP('',(#3704,#3705,#3706,#3707));
#1056=EDGE_LOOP('',(#3708,#3709,#3710,#3711));
#1057=EDGE_LOOP('',(#3712,#3713,#3714,#3715));
#1058=EDGE_LOOP('',(#3716));
#1059=EDGE_LOOP('',(#3717,#3718,#3719,#3720));
#1060=EDGE_LOOP('',(#3721));
#1061=EDGE_LOOP('',(#3722));
#1062=EDGE_LOOP('',(#3723,#3724,#3725,#3726));
#1063=EDGE_LOOP('',(#3727));
#1064=EDGE_LOOP('',(#3728,#3729,#3730,#3731));
#1065=EDGE_LOOP('',(#3732));
#1066=EDGE_LOOP('',(#3733));
#1067=EDGE_LOOP('',(#3734));
#1068=EDGE_LOOP('',(#3735));
#1069=EDGE_LOOP('',(#3736,#3737,#3738,#3739));
#1070=EDGE_LOOP('',(#3740));
#1071=EDGE_LOOP('',(#3741,#3742,#3743,#3744));
#1072=EDGE_LOOP('',(#3745));
#1073=EDGE_LOOP('',(#3746));
#1074=EDGE_LOOP('',(#3747));
#1075=EDGE_LOOP('',(#3748));
#1076=EDGE_LOOP('',(#3749));
#1077=EDGE_LOOP('',(#3750));
#1078=EDGE_LOOP('',(#3751));
#1079=EDGE_LOOP('',(#3752,#3753,#3754,#3755));
#1080=EDGE_LOOP('',(#3756,#3757,#3758,#3759));
#1081=EDGE_LOOP('',(#3760));
#1082=EDGE_LOOP('',(#3761));
#1083=EDGE_LOOP('',(#3762));
#1084=EDGE_LOOP('',(#3763));
#1085=EDGE_LOOP('',(#3764,#3765,#3766,#3767));
#1086=EDGE_LOOP('',(#3768,#3769,#3770,#3771));
#1087=EDGE_LOOP('',(#3772));
#1088=EDGE_LOOP('',(#3773));
#1089=EDGE_LOOP('',(#3774));
#1090=EDGE_LOOP('',(#3775));
#1091=EDGE_LOOP('',(#3776,#3777,#3778,#3779));
#1092=EDGE_LOOP('',(#3780,#3781,#3782,#3783));
#1093=EDGE_LOOP('',(#3784));
#1094=EDGE_LOOP('',(#3785));
#1095=EDGE_LOOP('',(#3786));
#1096=EDGE_LOOP('',(#3787));
#1097=EDGE_LOOP('',(#3788,#3789,#3790,#3791));
#1098=EDGE_LOOP('',(#3792,#3793,#3794,#3795));
#1099=EDGE_LOOP('',(#3796));
#1100=EDGE_LOOP('',(#3797));
#1101=EDGE_LOOP('',(#3798));
#1102=EDGE_LOOP('',(#3799));
#1103=EDGE_LOOP('',(#3800,#3801,#3802,#3803,#3804,#3805));
#1104=EDGE_LOOP('',(#3806));
#1105=EDGE_LOOP('',(#3807,#3808,#3809,#3810));
#1106=EDGE_LOOP('',(#3811,#3812,#3813,#3814));
#1107=EDGE_LOOP('',(#3815,#3816,#3817,#3818));
#1108=EDGE_LOOP('',(#3819,#3820,#3821,#3822));
#1109=EDGE_LOOP('',(#3823,#3824,#3825,#3826));
#1110=EDGE_LOOP('',(#3827,#3828,#3829,#3830));
#1111=EDGE_LOOP('',(#3831,#3832,#3833,#3834,#3835,#3836));
#1112=EDGE_LOOP('',(#3837,#3838,#3839,#3840));
#1113=EDGE_LOOP('',(#3841));
#1114=EDGE_LOOP('',(#3842,#3843,#3844,#3845));
#1115=EDGE_LOOP('',(#3846));
#1116=EDGE_LOOP('',(#3847));
#1117=EDGE_LOOP('',(#3848,#3849,#3850,#3851));
#1118=EDGE_LOOP('',(#3852));
#1119=EDGE_LOOP('',(#3853));
#1120=EDGE_LOOP('',(#3854,#3855,#3856,#3857));
#1121=EDGE_LOOP('',(#3858,#3859,#3860,#3861));
#1122=EDGE_LOOP('',(#3862,#3863,#3864,#3865));
#1123=EDGE_LOOP('',(#3866));
#1124=EDGE_LOOP('',(#3867));
#1125=EDGE_LOOP('',(#3868,#3869,#3870,#3871));
#1126=EDGE_LOOP('',(#3872,#3873,#3874,#3875));
#1127=EDGE_LOOP('',(#3876));
#1128=EDGE_LOOP('',(#3877));
#1129=EDGE_LOOP('',(#3878,#3879,#3880,#3881));
#1130=EDGE_LOOP('',(#3882,#3883,#3884,#3885));
#1131=EDGE_LOOP('',(#3886,#3887,#3888,#3889));
#1132=EDGE_LOOP('',(#3890,#3891,#3892,#3893));
#1133=EDGE_LOOP('',(#3894,#3895,#3896,#3897));
#1134=EDGE_LOOP('',(#3898,#3899,#3900,#3901));
#1135=EDGE_LOOP('',(#3902,#3903,#3904,#3905));
#1136=EDGE_LOOP('',(#3906,#3907,#3908,#3909));
#1137=EDGE_LOOP('',(#3910,#3911,#3912,#3913));
#1138=EDGE_LOOP('',(#3914,#3915,#3916,#3917,#3918,#3919));
#1139=EDGE_LOOP('',(#3920,#3921,#3922,#3923,#3924,#3925));
#1140=EDGE_LOOP('',(#3926));
#1141=EDGE_LOOP('',(#3927));
#1142=EDGE_LOOP('',(#3928,#3929,#3930,#3931));
#1143=EDGE_LOOP('',(#3932,#3933,#3934,#3935));
#1144=EDGE_LOOP('',(#3936,#3937,#3938,#3939));
#1145=EDGE_LOOP('',(#3940));
#1146=EDGE_LOOP('',(#3941));
#1147=EDGE_LOOP('',(#3942,#3943,#3944,#3945));
#1148=EDGE_LOOP('',(#3946,#3947,#3948,#3949));
#1149=EDGE_LOOP('',(#3950,#3951,#3952,#3953));
#1150=EDGE_LOOP('',(#3954));
#1151=EDGE_LOOP('',(#3955));
#1152=EDGE_LOOP('',(#3956,#3957,#3958,#3959,#3960,#3961));
#1153=EDGE_LOOP('',(#3962));
#1154=EDGE_LOOP('',(#3963,#3964,#3965,#3966,#3967,#3968));
#1155=EDGE_LOOP('',(#3969));
#1156=EDGE_LOOP('',(#3970,#3971,#3972,#3973));
#1157=EDGE_LOOP('',(#3974,#3975,#3976,#3977));
#1158=EDGE_LOOP('',(#3978,#3979,#3980,#3981));
#1159=EDGE_LOOP('',(#3982,#3983,#3984,#3985));
#1160=EDGE_LOOP('',(#3986,#3987,#3988,#3989));
#1161=EDGE_LOOP('',(#3990,#3991,#3992,#3993));
#1162=EDGE_LOOP('',(#3994));
#1163=EDGE_LOOP('',(#3995));
#1164=EDGE_LOOP('',(#3996,#3997,#3998,#3999));
#1165=EDGE_LOOP('',(#4000));
#1166=EDGE_LOOP('',(#4001));
#1167=EDGE_LOOP('',(#4002,#4003,#4004,#4005));
#1168=EDGE_LOOP('',(#4006,#4007,#4008,#4009));
#1169=EDGE_LOOP('',(#4010));
#1170=EDGE_LOOP('',(#4011));
#1171=EDGE_LOOP('',(#4012,#4013,#4014,#4015));
#1172=EDGE_LOOP('',(#4016));
#1173=EDGE_LOOP('',(#4017));
#1174=EDGE_LOOP('',(#4018,#4019,#4020,#4021));
#1175=EDGE_LOOP('',(#4022));
#1176=EDGE_LOOP('',(#4023));
#1177=EDGE_LOOP('',(#4024,#4025,#4026,#4027));
#1178=EDGE_LOOP('',(#4028));
#1179=EDGE_LOOP('',(#4029));
#1180=EDGE_LOOP('',(#4030,#4031,#4032,#4033));
#1181=EDGE_LOOP('',(#4034,#4035,#4036,#4037,#4038,#4039));
#1182=EDGE_LOOP('',(#4040));
#1183=EDGE_LOOP('',(#4041,#4042,#4043,#4044,#4045,#4046));
#1184=EDGE_LOOP('',(#4047));
#1185=EDGE_LOOP('',(#4048,#4049,#4050,#4051));
#1186=EDGE_LOOP('',(#4052,#4053,#4054,#4055));
#1187=EDGE_LOOP('',(#4056,#4057,#4058,#4059));
#1188=EDGE_LOOP('',(#4060,#4061,#4062,#4063));
#1189=EDGE_LOOP('',(#4064,#4065,#4066,#4067));
#1190=EDGE_LOOP('',(#4068,#4069,#4070,#4071));
#1191=EDGE_LOOP('',(#4072,#4073,#4074,#4075));
#1192=EDGE_LOOP('',(#4076));
#1193=EDGE_LOOP('',(#4077));
#1194=EDGE_LOOP('',(#4078,#4079,#4080,#4081));
#1195=EDGE_LOOP('',(#4082,#4083,#4084,#4085));
#1196=EDGE_LOOP('',(#4086,#4087,#4088,#4089));
#1197=EDGE_LOOP('',(#4090));
#1198=EDGE_LOOP('',(#4091));
#1199=EDGE_LOOP('',(#4092,#4093,#4094,#4095));
#1200=EDGE_LOOP('',(#4096));
#1201=EDGE_LOOP('',(#4097,#4098,#4099,#4100));
#1202=EDGE_LOOP('',(#4101,#4102,#4103,#4104));
#1203=EDGE_LOOP('',(#4105,#4106,#4107,#4108));
#1204=EDGE_LOOP('',(#4109));
#1205=EDGE_LOOP('',(#4110));
#1206=EDGE_LOOP('',(#4111,#4112,#4113,#4114));
#1207=EDGE_LOOP('',(#4115,#4116,#4117,#4118));
#1208=EDGE_LOOP('',(#4119,#4120,#4121,#4122));
#1209=EDGE_LOOP('',(#4123));
#1210=EDGE_LOOP('',(#4124,#4125,#4126,#4127));
#1211=EDGE_LOOP('',(#4128,#4129,#4130,#4131));
#1212=EDGE_LOOP('',(#4132,#4133,#4134,#4135));
#1213=EDGE_LOOP('',(#4136,#4137,#4138,#4139));
#1214=EDGE_LOOP('',(#4140,#4141,#4142,#4143));
#1215=EDGE_LOOP('',(#4144,#4145,#4146,#4147));
#1216=EDGE_LOOP('',(#4148,#4149,#4150,#4151,#4152,#4153));
#1217=EDGE_LOOP('',(#4154,#4155,#4156,#4157,#4158,#4159));
#1218=EDGE_LOOP('',(#4160,#4161,#4162,#4163));
#1219=EDGE_LOOP('',(#4164,#4165,#4166,#4167));
#1220=EDGE_LOOP('',(#4168,#4169,#4170,#4171));
#1221=EDGE_LOOP('',(#4172,#4173,#4174,#4175));
#1222=EDGE_LOOP('',(#4176,#4177,#4178,#4179));
#1223=EDGE_LOOP('',(#4180,#4181,#4182,#4183));
#1224=EDGE_LOOP('',(#4184,#4185,#4186,#4187,#4188,#4189));
#1225=EDGE_LOOP('',(#4190,#4191,#4192,#4193,#4194,#4195));
#1226=EDGE_LOOP('',(#4196));
#1227=EDGE_LOOP('',(#4197));
#1228=EDGE_LOOP('',(#4198,#4199,#4200,#4201));
#1229=EDGE_LOOP('',(#4202,#4203,#4204,#4205));
#1230=EDGE_LOOP('',(#4206,#4207,#4208,#4209));
#1231=EDGE_LOOP('',(#4210));
#1232=EDGE_LOOP('',(#4211));
#1233=EDGE_LOOP('',(#4212,#4213,#4214,#4215));
#1234=EDGE_LOOP('',(#4216,#4217,#4218,#4219));
#1235=LINE('',#6809,#1590);
#1236=LINE('',#6816,#1591);
#1237=LINE('',#6823,#1592);
#1238=LINE('',#6830,#1593);
#1239=LINE('',#6837,#1594);
#1240=LINE('',#6843,#1595);
#1241=LINE('',#6849,#1596);
#1242=LINE('',#6855,#1597);
#1243=LINE('',#6860,#1598);
#1244=LINE('',#6862,#1599);
#1245=LINE('',#6864,#1600);
#1246=LINE('',#6865,#1601);
#1247=LINE('',#6868,#1602);
#1248=LINE('',#6870,#1603);
#1249=LINE('',#6871,#1604);
#1250=LINE('',#6874,#1605);
#1251=LINE('',#6876,#1606);
#1252=LINE('',#6877,#1607);
#1253=LINE('',#6879,#1608);
#1254=LINE('',#6880,#1609);
#1255=LINE('',#6887,#1610);
#1256=LINE('',#6889,#1611);
#1257=LINE('',#6891,#1612);
#1258=LINE('',#6892,#1613);
#1259=LINE('',#6895,#1614);
#1260=LINE('',#6897,#1615);
#1261=LINE('',#6898,#1616);
#1262=LINE('',#6901,#1617);
#1263=LINE('',#6903,#1618);
#1264=LINE('',#6904,#1619);
#1265=LINE('',#6906,#1620);
#1266=LINE('',#6907,#1621);
#1267=LINE('',#6914,#1622);
#1268=LINE('',#6916,#1623);
#1269=LINE('',#6918,#1624);
#1270=LINE('',#6919,#1625);
#1271=LINE('',#6922,#1626);
#1272=LINE('',#6924,#1627);
#1273=LINE('',#6925,#1628);
#1274=LINE('',#6928,#1629);
#1275=LINE('',#6930,#1630);
#1276=LINE('',#6931,#1631);
#1277=LINE('',#6933,#1632);
#1278=LINE('',#6934,#1633);
#1279=LINE('',#6945,#1634);
#1280=LINE('',#6948,#1635);
#1281=LINE('',#6956,#1636);
#1282=LINE('',#6959,#1637);
#1283=LINE('',#6964,#1638);
#1284=LINE('',#6971,#1639);
#1285=LINE('',#6978,#1640);
#1286=LINE('',#6984,#1641);
#1287=LINE('',#6989,#1642);
#1288=LINE('',#6991,#1643);
#1289=LINE('',#6993,#1644);
#1290=LINE('',#6994,#1645);
#1291=LINE('',#6997,#1646);
#1292=LINE('',#6999,#1647);
#1293=LINE('',#7000,#1648);
#1294=LINE('',#7003,#1649);
#1295=LINE('',#7005,#1650);
#1296=LINE('',#7006,#1651);
#1297=LINE('',#7008,#1652);
#1298=LINE('',#7009,#1653);
#1299=LINE('',#7020,#1654);
#1300=LINE('',#7023,#1655);
#1301=LINE('',#7031,#1656);
#1302=LINE('',#7034,#1657);
#1303=LINE('',#7039,#1658);
#1304=LINE('',#7046,#1659);
#1305=LINE('',#7053,#1660);
#1306=LINE('',#7059,#1661);
#1307=LINE('',#7064,#1662);
#1308=LINE('',#7066,#1663);
#1309=LINE('',#7068,#1664);
#1310=LINE('',#7069,#1665);
#1311=LINE('',#7072,#1666);
#1312=LINE('',#7074,#1667);
#1313=LINE('',#7075,#1668);
#1314=LINE('',#7078,#1669);
#1315=LINE('',#7080,#1670);
#1316=LINE('',#7081,#1671);
#1317=LINE('',#7083,#1672);
#1318=LINE('',#7084,#1673);
#1319=LINE('',#7092,#1674);
#1320=LINE('',#7098,#1675);
#1321=LINE('',#7104,#1676);
#1322=LINE('',#7110,#1677);
#1323=LINE('',#7116,#1678);
#1324=LINE('',#7122,#1679);
#1325=LINE('',#7128,#1680);
#1326=LINE('',#7134,#1681);
#1327=LINE('',#7140,#1682);
#1328=LINE('',#7146,#1683);
#1329=LINE('',#7152,#1684);
#1330=LINE('',#7158,#1685);
#1331=LINE('',#7163,#1686);
#1332=LINE('',#7165,#1687);
#1333=LINE('',#7167,#1688);
#1334=LINE('',#7168,#1689);
#1335=LINE('',#7171,#1690);
#1336=LINE('',#7173,#1691);
#1337=LINE('',#7174,#1692);
#1338=LINE('',#7177,#1693);
#1339=LINE('',#7179,#1694);
#1340=LINE('',#7180,#1695);
#1341=LINE('',#7182,#1696);
#1342=LINE('',#7183,#1697);
#1343=LINE('',#7191,#1698);
#1344=LINE('',#7197,#1699);
#1345=LINE('',#7203,#1700);
#1346=LINE('',#7209,#1701);
#1347=LINE('',#7215,#1702);
#1348=LINE('',#7221,#1703);
#1349=LINE('',#7227,#1704);
#1350=LINE('',#7233,#1705);
#1351=LINE('',#7238,#1706);
#1352=LINE('',#7240,#1707);
#1353=LINE('',#7242,#1708);
#1354=LINE('',#7243,#1709);
#1355=LINE('',#7246,#1710);
#1356=LINE('',#7248,#1711);
#1357=LINE('',#7249,#1712);
#1358=LINE('',#7252,#1713);
#1359=LINE('',#7254,#1714);
#1360=LINE('',#7255,#1715);
#1361=LINE('',#7257,#1716);
#1362=LINE('',#7258,#1717);
#1363=LINE('',#7262,#1718);
#1364=LINE('',#7264,#1719);
#1365=LINE('',#7266,#1720);
#1366=LINE('',#7267,#1721);
#1367=LINE('',#7270,#1722);
#1368=LINE('',#7272,#1723);
#1369=LINE('',#7273,#1724);
#1370=LINE('',#7276,#1725);
#1371=LINE('',#7278,#1726);
#1372=LINE('',#7279,#1727);
#1373=LINE('',#7281,#1728);
#1374=LINE('',#7282,#1729);
#1375=LINE('',#7290,#1730);
#1376=LINE('',#7297,#1731);
#1377=LINE('',#7304,#1732);
#1378=LINE('',#7311,#1733);
#1379=LINE('',#7318,#1734);
#1380=LINE('',#7325,#1735);
#1381=LINE('',#7332,#1736);
#1382=LINE('',#7339,#1737);
#1383=LINE('',#7346,#1738);
#1384=LINE('',#7353,#1739);
#1385=LINE('',#7360,#1740);
#1386=LINE('',#7369,#1741);
#1387=LINE('',#7399,#1742);
#1388=LINE('',#7423,#1743);
#1389=LINE('',#7451,#1744);
#1390=LINE('',#7475,#1745);
#1391=LINE('',#7503,#1746);
#1392=LINE('',#7527,#1747);
#1393=LINE('',#7555,#1748);
#1394=LINE('',#7579,#1749);
#1395=LINE('',#7585,#1750);
#1396=LINE('',#7587,#1751);
#1397=LINE('',#7589,#1752);
#1398=LINE('',#7590,#1753);
#1399=LINE('',#7593,#1754);
#1400=LINE('',#7595,#1755);
#1401=LINE('',#7599,#1756);
#1402=LINE('',#7600,#1757);
#1403=LINE('',#7603,#1758);
#1404=LINE('',#7604,#1759);
#1405=LINE('',#7607,#1760);
#1406=LINE('',#7609,#1761);
#1407=LINE('',#7610,#1762);
#1408=LINE('',#7612,#1763);
#1409=LINE('',#7614,#1764);
#1410=LINE('',#7617,#1765);
#1411=LINE('',#7619,#1766);
#1412=LINE('',#7620,#1767);
#1413=LINE('',#7621,#1768);
#1414=LINE('',#7622,#1769);
#1415=LINE('',#7623,#1770);
#1416=LINE('',#7627,#1771);
#1417=LINE('',#7629,#1772);
#1418=LINE('',#7631,#1773);
#1419=LINE('',#7632,#1774);
#1420=LINE('',#7635,#1775);
#1421=LINE('',#7637,#1776);
#1422=LINE('',#7638,#1777);
#1423=LINE('',#7641,#1778);
#1424=LINE('',#7643,#1779);
#1425=LINE('',#7644,#1780);
#1426=LINE('',#7646,#1781);
#1427=LINE('',#7647,#1782);
#1428=LINE('',#7655,#1783);
#1429=LINE('',#7661,#1784);
#1430=LINE('',#7670,#1785);
#1431=LINE('',#7676,#1786);
#1432=LINE('',#7685,#1787);
#1433=LINE('',#7691,#1788);
#1434=LINE('',#7700,#1789);
#1435=LINE('',#7706,#1790);
#1436=LINE('',#7714,#1791);
#1437=LINE('',#7716,#1792);
#1438=LINE('',#7718,#1793);
#1439=LINE('',#7720,#1794);
#1440=LINE('',#7722,#1795);
#1441=LINE('',#7723,#1796);
#1442=LINE('',#7728,#1797);
#1443=LINE('',#7730,#1798);
#1444=LINE('',#7731,#1799);
#1445=LINE('',#7734,#1800);
#1446=LINE('',#7735,#1801);
#1447=LINE('',#7738,#1802);
#1448=LINE('',#7739,#1803);
#1449=LINE('',#7742,#1804);
#1450=LINE('',#7743,#1805);
#1451=LINE('',#7746,#1806);
#1452=LINE('',#7747,#1807);
#1453=LINE('',#7749,#1808);
#1454=LINE('',#7753,#1809);
#1455=LINE('',#7761,#1810);
#1456=LINE('',#7770,#1811);
#1457=LINE('',#7779,#1812);
#1458=LINE('',#7785,#1813);
#1459=LINE('',#7790,#1814);
#1460=LINE('',#7792,#1815);
#1461=LINE('',#7794,#1816);
#1462=LINE('',#7795,#1817);
#1463=LINE('',#7798,#1818);
#1464=LINE('',#7800,#1819);
#1465=LINE('',#7801,#1820);
#1466=LINE('',#7804,#1821);
#1467=LINE('',#7806,#1822);
#1468=LINE('',#7807,#1823);
#1469=LINE('',#7809,#1824);
#1470=LINE('',#7810,#1825);
#1471=LINE('',#7817,#1826);
#1472=LINE('',#7819,#1827);
#1473=LINE('',#7821,#1828);
#1474=LINE('',#7822,#1829);
#1475=LINE('',#7825,#1830);
#1476=LINE('',#7827,#1831);
#1477=LINE('',#7828,#1832);
#1478=LINE('',#7831,#1833);
#1479=LINE('',#7833,#1834);
#1480=LINE('',#7834,#1835);
#1481=LINE('',#7837,#1836);
#1482=LINE('',#7839,#1837);
#1483=LINE('',#7840,#1838);
#1484=LINE('',#7843,#1839);
#1485=LINE('',#7845,#1840);
#1486=LINE('',#7846,#1841);
#1487=LINE('',#7848,#1842);
#1488=LINE('',#7849,#1843);
#1489=LINE('',#7861,#1844);
#1490=LINE('',#7865,#1845);
#1491=LINE('',#7869,#1846);
#1492=LINE('',#7876,#1847);
#1493=LINE('',#7878,#1848);
#1494=LINE('',#7885,#1849);
#1495=LINE('',#7893,#1850);
#1496=LINE('',#7895,#1851);
#1497=LINE('',#7897,#1852);
#1498=LINE('',#7899,#1853);
#1499=LINE('',#7901,#1854);
#1500=LINE('',#7902,#1855);
#1501=LINE('',#7908,#1856);
#1502=LINE('',#7910,#1857);
#1503=LINE('',#7912,#1858);
#1504=LINE('',#7914,#1859);
#1505=LINE('',#7916,#1860);
#1506=LINE('',#7917,#1861);
#1507=LINE('',#7921,#1862);
#1508=LINE('',#7922,#1863);
#1509=LINE('',#7924,#1864);
#1510=LINE('',#7926,#1865);
#1511=LINE('',#7928,#1866);
#1512=LINE('',#7930,#1867);
#1513=LINE('',#7937,#1868);
#1514=LINE('',#7943,#1869);
#1515=LINE('',#7947,#1870);
#1516=LINE('',#7952,#1871);
#1517=LINE('',#7962,#1872);
#1518=LINE('',#7969,#1873);
#1519=LINE('',#7974,#1874);
#1520=LINE('',#7981,#1875);
#1521=LINE('',#7983,#1876);
#1522=LINE('',#7985,#1877);
#1523=LINE('',#7987,#1878);
#1524=LINE('',#7989,#1879);
#1525=LINE('',#7990,#1880);
#1526=LINE('',#7996,#1881);
#1527=LINE('',#7998,#1882);
#1528=LINE('',#8000,#1883);
#1529=LINE('',#8002,#1884);
#1530=LINE('',#8004,#1885);
#1531=LINE('',#8005,#1886);
#1532=LINE('',#8009,#1887);
#1533=LINE('',#8010,#1888);
#1534=LINE('',#8012,#1889);
#1535=LINE('',#8014,#1890);
#1536=LINE('',#8016,#1891);
#1537=LINE('',#8018,#1892);
#1538=LINE('',#8022,#1893);
#1539=LINE('',#8030,#1894);
#1540=LINE('',#8034,#1895);
#1541=LINE('',#8038,#1896);
#1542=LINE('',#8043,#1897);
#1543=LINE('',#8051,#1898);
#1544=LINE('',#8055,#1899);
#1545=LINE('',#8059,#1900);
#1546=LINE('',#8066,#1901);
#1547=LINE('',#8070,#1902);
#1548=LINE('',#8074,#1903);
#1549=LINE('',#8079,#1904);
#1550=LINE('',#8081,#1905);
#1551=LINE('',#8083,#1906);
#1552=LINE('',#8084,#1907);
#1553=LINE('',#8087,#1908);
#1554=LINE('',#8089,#1909);
#1555=LINE('',#8090,#1910);
#1556=LINE('',#8093,#1911);
#1557=LINE('',#8095,#1912);
#1558=LINE('',#8096,#1913);
#1559=LINE('',#8099,#1914);
#1560=LINE('',#8101,#1915);
#1561=LINE('',#8102,#1916);
#1562=LINE('',#8105,#1917);
#1563=LINE('',#8107,#1918);
#1564=LINE('',#8108,#1919);
#1565=LINE('',#8110,#1920);
#1566=LINE('',#8111,#1921);
#1567=LINE('',#8118,#1922);
#1568=LINE('',#8120,#1923);
#1569=LINE('',#8122,#1924);
#1570=LINE('',#8123,#1925);
#1571=LINE('',#8126,#1926);
#1572=LINE('',#8128,#1927);
#1573=LINE('',#8129,#1928);
#1574=LINE('',#8132,#1929);
#1575=LINE('',#8134,#1930);
#1576=LINE('',#8135,#1931);
#1577=LINE('',#8138,#1932);
#1578=LINE('',#8140,#1933);
#1579=LINE('',#8141,#1934);
#1580=LINE('',#8144,#1935);
#1581=LINE('',#8146,#1936);
#1582=LINE('',#8147,#1937);
#1583=LINE('',#8149,#1938);
#1584=LINE('',#8150,#1939);
#1585=LINE('',#8162,#1940);
#1586=LINE('',#8166,#1941);
#1587=LINE('',#8170,#1942);
#1588=LINE('',#8177,#1943);
#1589=LINE('',#8179,#1944);
#1590=VECTOR('',#5390,0.5);
#1591=VECTOR('',#5399,0.5);
#1592=VECTOR('',#5408,0.5);
#1593=VECTOR('',#5417,0.5);
#1594=VECTOR('',#5426,0.21);
#1595=VECTOR('',#5433,0.21);
#1596=VECTOR('',#5440,0.21);
#1597=VECTOR('',#5447,0.21);
#1598=VECTOR('',#5452,1.);
#1599=VECTOR('',#5453,1.);
#1600=VECTOR('',#5454,1.);
#1601=VECTOR('',#5455,1.);
#1602=VECTOR('',#5458,1.);
#1603=VECTOR('',#5459,1.);
#1604=VECTOR('',#5460,1.);
#1605=VECTOR('',#5463,1.);
#1606=VECTOR('',#5464,1.);
#1607=VECTOR('',#5465,1.);
#1608=VECTOR('',#5468,1.);
#1609=VECTOR('',#5469,1.);
#1610=VECTOR('',#5478,1.);
#1611=VECTOR('',#5479,1.);
#1612=VECTOR('',#5480,1.);
#1613=VECTOR('',#5481,1.);
#1614=VECTOR('',#5484,1.);
#1615=VECTOR('',#5485,1.);
#1616=VECTOR('',#5486,1.);
#1617=VECTOR('',#5489,1.);
#1618=VECTOR('',#5490,1.);
#1619=VECTOR('',#5491,1.);
#1620=VECTOR('',#5494,1.);
#1621=VECTOR('',#5495,1.);
#1622=VECTOR('',#5504,1.);
#1623=VECTOR('',#5505,1.);
#1624=VECTOR('',#5506,1.);
#1625=VECTOR('',#5507,1.);
#1626=VECTOR('',#5510,1.);
#1627=VECTOR('',#5511,1.);
#1628=VECTOR('',#5512,1.);
#1629=VECTOR('',#5515,1.);
#1630=VECTOR('',#5516,1.);
#1631=VECTOR('',#5517,1.);
#1632=VECTOR('',#5520,1.);
#1633=VECTOR('',#5521,1.);
#1634=VECTOR('',#5536,1.);
#1635=VECTOR('',#5539,1.);
#1636=VECTOR('',#5548,1.);
#1637=VECTOR('',#5551,1.);
#1638=VECTOR('',#5556,0.275);
#1639=VECTOR('',#5565,0.275);
#1640=VECTOR('',#5574,0.275);
#1641=VECTOR('',#5581,0.275);
#1642=VECTOR('',#5586,1.);
#1643=VECTOR('',#5587,1.);
#1644=VECTOR('',#5588,1.);
#1645=VECTOR('',#5589,1.);
#1646=VECTOR('',#5592,1.);
#1647=VECTOR('',#5593,1.);
#1648=VECTOR('',#5594,1.);
#1649=VECTOR('',#5597,1.);
#1650=VECTOR('',#5598,1.);
#1651=VECTOR('',#5599,1.);
#1652=VECTOR('',#5602,1.);
#1653=VECTOR('',#5603,1.);
#1654=VECTOR('',#5618,1.);
#1655=VECTOR('',#5621,1.);
#1656=VECTOR('',#5630,1.);
#1657=VECTOR('',#5633,1.);
#1658=VECTOR('',#5638,0.275);
#1659=VECTOR('',#5647,0.275);
#1660=VECTOR('',#5656,0.275);
#1661=VECTOR('',#5663,0.275);
#1662=VECTOR('',#5668,1.);
#1663=VECTOR('',#5669,1.);
#1664=VECTOR('',#5670,1.);
#1665=VECTOR('',#5671,1.);
#1666=VECTOR('',#5674,1.);
#1667=VECTOR('',#5675,1.);
#1668=VECTOR('',#5676,1.);
#1669=VECTOR('',#5679,1.);
#1670=VECTOR('',#5680,1.);
#1671=VECTOR('',#5681,1.);
#1672=VECTOR('',#5684,1.);
#1673=VECTOR('',#5685,1.);
#1674=VECTOR('',#5696,0.15);
#1675=VECTOR('',#5703,0.15);
#1676=VECTOR('',#5710,0.225);
#1677=VECTOR('',#5717,0.225);
#1678=VECTOR('',#5724,0.225);
#1679=VECTOR('',#5731,0.225);
#1680=VECTOR('',#5738,0.225);
#1681=VECTOR('',#5745,0.225);
#1682=VECTOR('',#5752,0.21);
#1683=VECTOR('',#5759,0.21);
#1684=VECTOR('',#5766,0.21);
#1685=VECTOR('',#5773,0.21);
#1686=VECTOR('',#5778,1.);
#1687=VECTOR('',#5779,1.);
#1688=VECTOR('',#5780,1.);
#1689=VECTOR('',#5781,1.);
#1690=VECTOR('',#5784,1.);
#1691=VECTOR('',#5785,1.);
#1692=VECTOR('',#5786,1.);
#1693=VECTOR('',#5789,1.);
#1694=VECTOR('',#5790,1.);
#1695=VECTOR('',#5791,1.);
#1696=VECTOR('',#5794,1.);
#1697=VECTOR('',#5795,1.);
#1698=VECTOR('',#5806,0.15);
#1699=VECTOR('',#5813,0.15);
#1700=VECTOR('',#5820,0.225);
#1701=VECTOR('',#5827,0.225);
#1702=VECTOR('',#5834,0.225);
#1703=VECTOR('',#5841,0.225);
#1704=VECTOR('',#5848,0.225);
#1705=VECTOR('',#5855,0.225);
#1706=VECTOR('',#5860,1.);
#1707=VECTOR('',#5861,1.);
#1708=VECTOR('',#5862,1.);
#1709=VECTOR('',#5863,1.);
#1710=VECTOR('',#5866,1.);
#1711=VECTOR('',#5867,1.);
#1712=VECTOR('',#5868,1.);
#1713=VECTOR('',#5871,1.);
#1714=VECTOR('',#5872,1.);
#1715=VECTOR('',#5873,1.);
#1716=VECTOR('',#5876,1.);
#1717=VECTOR('',#5877,1.);
#1718=VECTOR('',#5880,1.);
#1719=VECTOR('',#5881,1.);
#1720=VECTOR('',#5882,1.);
#1721=VECTOR('',#5883,1.);
#1722=VECTOR('',#5886,1.);
#1723=VECTOR('',#5887,1.);
#1724=VECTOR('',#5888,1.);
#1725=VECTOR('',#5891,1.);
#1726=VECTOR('',#5892,1.);
#1727=VECTOR('',#5893,1.);
#1728=VECTOR('',#5896,1.);
#1729=VECTOR('',#5897,1.);
#1730=VECTOR('',#5908,0.165);
#1731=VECTOR('',#5917,0.165);
#1732=VECTOR('',#5926,0.15);
#1733=VECTOR('',#5935,0.15);
#1734=VECTOR('',#5944,0.165);
#1735=VECTOR('',#5953,0.165);
#1736=VECTOR('',#5962,0.165);
#1737=VECTOR('',#5971,0.165);
#1738=VECTOR('',#5980,0.165);
#1739=VECTOR('',#5989,0.165);
#1740=VECTOR('',#5998,0.685);
#1741=VECTOR('',#6009,0.685);
#1742=VECTOR('',#6018,0.2);
#1743=VECTOR('',#6025,0.515);
#1744=VECTOR('',#6032,0.2);
#1745=VECTOR('',#6039,0.515);
#1746=VECTOR('',#6046,0.2);
#1747=VECTOR('',#6053,0.515);
#1748=VECTOR('',#6060,0.2);
#1749=VECTOR('',#6067,0.515);
#1750=VECTOR('',#6074,1.);
#1751=VECTOR('',#6075,1.);
#1752=VECTOR('',#6076,1.);
#1753=VECTOR('',#6077,1.);
#1754=VECTOR('',#6080,1.);
#1755=VECTOR('',#6081,1.);
#1756=VECTOR('',#6084,1.);
#1757=VECTOR('',#6085,1.);
#1758=VECTOR('',#6088,1.);
#1759=VECTOR('',#6089,1.);
#1760=VECTOR('',#6092,1.);
#1761=VECTOR('',#6093,1.);
#1762=VECTOR('',#6094,1.);
#1763=VECTOR('',#6097,1.);
#1764=VECTOR('',#6098,1.);
#1765=VECTOR('',#6103,1.);
#1766=VECTOR('',#6106,0.3);
#1767=VECTOR('',#6107,0.3);
#1768=VECTOR('',#6108,0.3);
#1769=VECTOR('',#6109,0.3);
#1770=VECTOR('',#6110,0.3);
#1771=VECTOR('',#6113,1.);
#1772=VECTOR('',#6114,1.);
#1773=VECTOR('',#6115,1.);
#1774=VECTOR('',#6116,1.);
#1775=VECTOR('',#6119,1.);
#1776=VECTOR('',#6120,1.);
#1777=VECTOR('',#6121,1.);
#1778=VECTOR('',#6124,1.);
#1779=VECTOR('',#6125,1.);
#1780=VECTOR('',#6126,1.);
#1781=VECTOR('',#6129,1.);
#1782=VECTOR('',#6130,1.);
#1783=VECTOR('',#6141,0.2);
#1784=VECTOR('',#6148,0.3);
#1785=VECTOR('',#6161,0.2);
#1786=VECTOR('',#6168,0.3);
#1787=VECTOR('',#6181,0.2);
#1788=VECTOR('',#6188,0.3);
#1789=VECTOR('',#6201,0.2);
#1790=VECTOR('',#6208,0.3);
#1791=VECTOR('',#6219,1.);
#1792=VECTOR('',#6220,1.);
#1793=VECTOR('',#6221,1.);
#1794=VECTOR('',#6222,1.);
#1795=VECTOR('',#6223,1.);
#1796=VECTOR('',#6224,1.);
#1797=VECTOR('',#6229,1.);
#1798=VECTOR('',#6230,1.);
#1799=VECTOR('',#6231,1.);
#1800=VECTOR('',#6234,1.);
#1801=VECTOR('',#6235,1.);
#1802=VECTOR('',#6238,1.);
#1803=VECTOR('',#6239,1.);
#1804=VECTOR('',#6242,1.);
#1805=VECTOR('',#6243,1.);
#1806=VECTOR('',#6246,1.);
#1807=VECTOR('',#6247,1.);
#1808=VECTOR('',#6250,1.);
#1809=VECTOR('',#6255,0.685);
#1810=VECTOR('',#6266,0.15);
#1811=VECTOR('',#6279,0.15);
#1812=VECTOR('',#6292,0.225);
#1813=VECTOR('',#6299,0.225);
#1814=VECTOR('',#6304,1.);
#1815=VECTOR('',#6305,1.);
#1816=VECTOR('',#6306,1.);
#1817=VECTOR('',#6307,1.);
#1818=VECTOR('',#6310,1.);
#1819=VECTOR('',#6311,1.);
#1820=VECTOR('',#6312,1.);
#1821=VECTOR('',#6315,1.);
#1822=VECTOR('',#6316,1.);
#1823=VECTOR('',#6317,1.);
#1824=VECTOR('',#6320,1.);
#1825=VECTOR('',#6321,1.);
#1826=VECTOR('',#6330,1.);
#1827=VECTOR('',#6331,1.);
#1828=VECTOR('',#6332,1.);
#1829=VECTOR('',#6333,1.);
#1830=VECTOR('',#6336,1.);
#1831=VECTOR('',#6337,1.);
#1832=VECTOR('',#6338,1.);
#1833=VECTOR('',#6341,1.);
#1834=VECTOR('',#6342,1.);
#1835=VECTOR('',#6343,1.);
#1836=VECTOR('',#6346,1.);
#1837=VECTOR('',#6347,1.);
#1838=VECTOR('',#6348,1.);
#1839=VECTOR('',#6351,1.);
#1840=VECTOR('',#6352,1.);
#1841=VECTOR('',#6353,1.);
#1842=VECTOR('',#6356,1.);
#1843=VECTOR('',#6357,1.);
#1844=VECTOR('',#6374,0.4);
#1845=VECTOR('',#6379,0.425);
#1846=VECTOR('',#6384,0.41);
#1847=VECTOR('',#6393,0.26);
#1848=VECTOR('',#6396,0.25);
#1849=VECTOR('',#6405,0.43);
#1850=VECTOR('',#6414,1.);
#1851=VECTOR('',#6415,1.);
#1852=VECTOR('',#6416,1.);
#1853=VECTOR('',#6417,1.);
#1854=VECTOR('',#6418,1.);
#1855=VECTOR('',#6419,1.);
#1856=VECTOR('',#6424,1.);
#1857=VECTOR('',#6425,1.);
#1858=VECTOR('',#6426,1.);
#1859=VECTOR('',#6427,1.);
#1860=VECTOR('',#6428,1.);
#1861=VECTOR('',#6429,1.);
#1862=VECTOR('',#6434,1.);
#1863=VECTOR('',#6435,1.);
#1864=VECTOR('',#6438,1.);
#1865=VECTOR('',#6441,1.);
#1866=VECTOR('',#6444,1.);
#1867=VECTOR('',#6447,1.);
#1868=VECTOR('',#6456,0.46);
#1869=VECTOR('',#6465,0.525);
#1870=VECTOR('',#6470,0.515);
#1871=VECTOR('',#6477,0.2);
#1872=VECTOR('',#6490,0.475);
#1873=VECTOR('',#6499,0.355);
#1874=VECTOR('',#6506,0.31);
#1875=VECTOR('',#6515,1.);
#1876=VECTOR('',#6516,1.);
#1877=VECTOR('',#6517,1.);
#1878=VECTOR('',#6518,1.);
#1879=VECTOR('',#6519,1.);
#1880=VECTOR('',#6520,1.);
#1881=VECTOR('',#6525,1.);
#1882=VECTOR('',#6526,1.);
#1883=VECTOR('',#6527,1.);
#1884=VECTOR('',#6528,1.);
#1885=VECTOR('',#6529,1.);
#1886=VECTOR('',#6530,1.);
#1887=VECTOR('',#6535,1.);
#1888=VECTOR('',#6536,1.);
#1889=VECTOR('',#6539,1.);
#1890=VECTOR('',#6542,1.);
#1891=VECTOR('',#6545,1.);
#1892=VECTOR('',#6548,1.);
#1893=VECTOR('',#6553,0.685);
#1894=VECTOR('',#6564,0.645);
#1895=VECTOR('',#6569,0.685);
#1896=VECTOR('',#6574,0.645);
#1897=VECTOR('',#6581,0.46);
#1898=VECTOR('',#6592,0.325);
#1899=VECTOR('',#6597,0.35);
#1900=VECTOR('',#6602,0.335);
#1901=VECTOR('',#6611,0.21);
#1902=VECTOR('',#6616,0.2);
#1903=VECTOR('',#6621,0.18);
#1904=VECTOR('',#6626,1.);
#1905=VECTOR('',#6627,1.);
#1906=VECTOR('',#6628,1.);
#1907=VECTOR('',#6629,1.);
#1908=VECTOR('',#6632,1.);
#1909=VECTOR('',#6633,1.);
#1910=VECTOR('',#6634,1.);
#1911=VECTOR('',#6637,1.);
#1912=VECTOR('',#6638,1.);
#1913=VECTOR('',#6639,1.);
#1914=VECTOR('',#6642,1.);
#1915=VECTOR('',#6643,1.);
#1916=VECTOR('',#6644,1.);
#1917=VECTOR('',#6647,1.);
#1918=VECTOR('',#6648,1.);
#1919=VECTOR('',#6649,1.);
#1920=VECTOR('',#6652,1.);
#1921=VECTOR('',#6653,1.);
#1922=VECTOR('',#6662,1.);
#1923=VECTOR('',#6663,1.);
#1924=VECTOR('',#6664,1.);
#1925=VECTOR('',#6665,1.);
#1926=VECTOR('',#6668,1.);
#1927=VECTOR('',#6669,1.);
#1928=VECTOR('',#6670,1.);
#1929=VECTOR('',#6673,1.);
#1930=VECTOR('',#6674,1.);
#1931=VECTOR('',#6675,1.);
#1932=VECTOR('',#6678,1.);
#1933=VECTOR('',#6679,1.);
#1934=VECTOR('',#6680,1.);
#1935=VECTOR('',#6683,1.);
#1936=VECTOR('',#6684,1.);
#1937=VECTOR('',#6685,1.);
#1938=VECTOR('',#6688,1.);
#1939=VECTOR('',#6689,1.);
#1940=VECTOR('',#6706,0.325);
#1941=VECTOR('',#6711,0.35);
#1942=VECTOR('',#6716,0.335);
#1943=VECTOR('',#6725,0.21);
#1944=VECTOR('',#6728,0.2);
#1945=CIRCLE('',#4852,0.5);
#1946=CIRCLE('',#4853,0.5);
#1947=CIRCLE('',#4856,0.5);
#1948=CIRCLE('',#4857,0.5);
#1949=CIRCLE('',#4860,0.5);
#1950=CIRCLE('',#4861,0.5);
#1951=CIRCLE('',#4864,0.5);
#1952=CIRCLE('',#4865,0.5);
#1953=CIRCLE('',#4868,0.21);
#1954=CIRCLE('',#4869,0.21);
#1955=CIRCLE('',#4871,0.21);
#1956=CIRCLE('',#4872,0.21);
#1957=CIRCLE('',#4874,0.21);
#1958=CIRCLE('',#4875,0.21);
#1959=CIRCLE('',#4877,0.21);
#1960=CIRCLE('',#4878,0.21);
#1961=CIRCLE('',#4901,0.275);
#1962=CIRCLE('',#4902,0.45);
#1963=CIRCLE('',#4904,0.45);
#1964=CIRCLE('',#4906,0.275);
#1965=CIRCLE('',#4907,0.45);
#1966=CIRCLE('',#4909,0.45);
#1967=CIRCLE('',#4911,0.275);
#1968=CIRCLE('',#4912,0.275);
#1969=CIRCLE('',#4913,0.275);
#1970=CIRCLE('',#4915,0.275);
#1971=CIRCLE('',#4916,0.275);
#1972=CIRCLE('',#4917,0.275);
#1973=CIRCLE('',#4919,0.275);
#1974=CIRCLE('',#4920,0.275);
#1975=CIRCLE('',#4922,0.275);
#1976=CIRCLE('',#4923,0.275);
#1977=CIRCLE('',#4932,0.275);
#1978=CIRCLE('',#4933,0.45);
#1979=CIRCLE('',#4935,0.45);
#1980=CIRCLE('',#4937,0.275);
#1981=CIRCLE('',#4938,0.45);
#1982=CIRCLE('',#4940,0.45);
#1983=CIRCLE('',#4942,0.275);
#1984=CIRCLE('',#4943,0.275);
#1985=CIRCLE('',#4944,0.275);
#1986=CIRCLE('',#4946,0.275);
#1987=CIRCLE('',#4947,0.275);
#1988=CIRCLE('',#4948,0.275);
#1989=CIRCLE('',#4950,0.275);
#1990=CIRCLE('',#4951,0.275);
#1991=CIRCLE('',#4953,0.275);
#1992=CIRCLE('',#4954,0.275);
#1993=CIRCLE('',#4963,0.15);
#1994=CIRCLE('',#4964,0.15);
#1995=CIRCLE('',#4966,0.15);
#1996=CIRCLE('',#4967,0.15);
#1997=CIRCLE('',#4969,0.225);
#1998=CIRCLE('',#4970,0.225);
#1999=CIRCLE('',#4972,0.225);
#2000=CIRCLE('',#4973,0.225);
#2001=CIRCLE('',#4975,0.225);
#2002=CIRCLE('',#4976,0.225);
#2003=CIRCLE('',#4978,0.225);
#2004=CIRCLE('',#4979,0.225);
#2005=CIRCLE('',#4981,0.225);
#2006=CIRCLE('',#4982,0.225);
#2007=CIRCLE('',#4984,0.225);
#2008=CIRCLE('',#4985,0.225);
#2009=CIRCLE('',#4987,0.21);
#2010=CIRCLE('',#4988,0.21);
#2011=CIRCLE('',#4990,0.21);
#2012=CIRCLE('',#4991,0.21);
#2013=CIRCLE('',#4993,0.21);
#2014=CIRCLE('',#4994,0.21);
#2015=CIRCLE('',#4996,0.21);
#2016=CIRCLE('',#4997,0.21);
#2017=CIRCLE('',#5006,0.15);
#2018=CIRCLE('',#5007,0.15);
#2019=CIRCLE('',#5009,0.15);
#2020=CIRCLE('',#5010,0.15);
#2021=CIRCLE('',#5012,0.225);
#2022=CIRCLE('',#5013,0.225);
#2023=CIRCLE('',#5015,0.225);
#2024=CIRCLE('',#5016,0.225);
#2025=CIRCLE('',#5018,0.225);
#2026=CIRCLE('',#5019,0.225);
#2027=CIRCLE('',#5021,0.225);
#2028=CIRCLE('',#5022,0.225);
#2029=CIRCLE('',#5024,0.225);
#2030=CIRCLE('',#5025,0.225);
#2031=CIRCLE('',#5027,0.225);
#2032=CIRCLE('',#5028,0.225);
#2033=CIRCLE('',#5041,0.165);
#2034=CIRCLE('',#5042,0.165);
#2035=CIRCLE('',#5045,0.165);
#2036=CIRCLE('',#5046,0.165);
#2037=CIRCLE('',#5049,0.15);
#2038=CIRCLE('',#5050,0.15);
#2039=CIRCLE('',#5053,0.15);
#2040=CIRCLE('',#5054,0.15);
#2041=CIRCLE('',#5057,0.165);
#2042=CIRCLE('',#5058,0.165);
#2043=CIRCLE('',#5061,0.165);
#2044=CIRCLE('',#5062,0.165);
#2045=CIRCLE('',#5065,0.165);
#2046=CIRCLE('',#5066,0.165);
#2047=CIRCLE('',#5069,0.165);
#2048=CIRCLE('',#5070,0.165);
#2049=CIRCLE('',#5073,0.165);
#2050=CIRCLE('',#5074,0.165);
#2051=CIRCLE('',#5077,0.165);
#2052=CIRCLE('',#5078,0.165);
#2053=CIRCLE('',#5081,0.685);
#2054=CIRCLE('',#5082,0.685);
#2055=CIRCLE('',#5084,0.3);
#2056=CIRCLE('',#5086,0.685);
#2057=CIRCLE('',#5087,0.685);
#2058=CIRCLE('',#5089,0.3);
#2059=CIRCLE('',#5091,0.2);
#2060=CIRCLE('',#5093,0.515);
#2061=CIRCLE('',#5094,0.515);
#2062=CIRCLE('',#5097,0.2);
#2063=CIRCLE('',#5099,0.515);
#2064=CIRCLE('',#5100,0.515);
#2065=CIRCLE('',#5103,0.2);
#2066=CIRCLE('',#5105,0.515);
#2067=CIRCLE('',#5106,0.515);
#2068=CIRCLE('',#5109,0.2);
#2069=CIRCLE('',#5111,0.515);
#2070=CIRCLE('',#5112,0.515);
#2071=CIRCLE('',#5116,0.3);
#2072=CIRCLE('',#5120,0.3);
#2073=CIRCLE('',#5131,0.2);
#2074=CIRCLE('',#5132,0.2);
#2075=CIRCLE('',#5134,0.3);
#2076=CIRCLE('',#5135,0.3);
#2077=CIRCLE('',#5140,0.2);
#2078=CIRCLE('',#5141,0.2);
#2079=CIRCLE('',#5143,0.3);
#2080=CIRCLE('',#5144,0.3);
#2081=CIRCLE('',#5149,0.2);
#2082=CIRCLE('',#5150,0.2);
#2083=CIRCLE('',#5152,0.3);
#2084=CIRCLE('',#5153,0.3);
#2085=CIRCLE('',#5158,0.2);
#2086=CIRCLE('',#5159,0.2);
#2087=CIRCLE('',#5161,0.3);
#2088=CIRCLE('',#5162,0.3);
#2089=CIRCLE('',#5167,0.685);
#2090=CIRCLE('',#5176,0.685);
#2091=CIRCLE('',#5180,0.15);
#2092=CIRCLE('',#5181,0.15);
#2093=CIRCLE('',#5186,0.15);
#2094=CIRCLE('',#5187,0.15);
#2095=CIRCLE('',#5192,0.225);
#2096=CIRCLE('',#5193,0.225);
#2097=CIRCLE('',#5195,0.225);
#2098=CIRCLE('',#5196,0.225);
#2099=CIRCLE('',#5213,0.24505);
#2100=CIRCLE('',#5215,0.375);
#2101=CIRCLE('',#5217,0.425);
#2102=CIRCLE('',#5219,0.425);
#2103=CIRCLE('',#5221,0.395);
#2104=CIRCLE('',#5223,0.27);
#2105=CIRCLE('',#5225,0.24505);
#2106=CIRCLE('',#5230,0.43);
#2107=CIRCLE('',#5231,0.43);
#2108=CIRCLE('',#5233,0.2);
#2109=CIRCLE('',#5235,0.525);
#2110=CIRCLE('',#5237,0.515);
#2111=CIRCLE('',#5245,0.46);
#2112=CIRCLE('',#5247,0.46);
#2113=CIRCLE('',#5249,0.525);
#2114=CIRCLE('',#5252,0.515);
#2115=CIRCLE('',#5254,0.2);
#2116=CIRCLE('',#5258,0.475);
#2117=CIRCLE('',#5259,0.31);
#2118=CIRCLE('',#5261,0.475);
#2119=CIRCLE('',#5263,0.355);
#2120=CIRCLE('',#5265,0.355);
#2121=CIRCLE('',#5267,0.31);
#2122=CIRCLE('',#5273,0.685);
#2123=CIRCLE('',#5275,0.685);
#2124=CIRCLE('',#5283,0.685);
#2125=CIRCLE('',#5285,0.605);
#2126=CIRCLE('',#5286,0.46);
#2127=CIRCLE('',#5289,0.685);
#2128=CIRCLE('',#5291,0.605);
#2129=CIRCLE('',#5293,0.46);
#2130=CIRCLE('',#5297,0.3);
#2131=CIRCLE('',#5299,0.35);
#2132=CIRCLE('',#5301,0.35);
#2133=CIRCLE('',#5303,0.32);
#2134=CIRCLE('',#5305,0.22);
#2135=CIRCLE('',#5307,0.1954);
#2136=CIRCLE('',#5309,0.1954);
#2137=CIRCLE('',#5311,0.16);
#2138=CIRCLE('',#5331,0.1954);
#2139=CIRCLE('',#5333,0.3);
#2140=CIRCLE('',#5335,0.35);
#2141=CIRCLE('',#5337,0.35);
#2142=CIRCLE('',#5339,0.32);
#2143=CIRCLE('',#5341,0.22);
#2144=CIRCLE('',#5343,0.1954);
#2145=VERTEX_POINT('',#6806);
#2146=VERTEX_POINT('',#6808);
#2147=VERTEX_POINT('',#6813);
#2148=VERTEX_POINT('',#6815);
#2149=VERTEX_POINT('',#6820);
#2150=VERTEX_POINT('',#6822);
#2151=VERTEX_POINT('',#6827);
#2152=VERTEX_POINT('',#6829);
#2153=VERTEX_POINT('',#6834);
#2154=VERTEX_POINT('',#6836);
#2155=VERTEX_POINT('',#6840);
#2156=VERTEX_POINT('',#6842);
#2157=VERTEX_POINT('',#6846);
#2158=VERTEX_POINT('',#6848);
#2159=VERTEX_POINT('',#6852);
#2160=VERTEX_POINT('',#6854);
#2161=VERTEX_POINT('',#6858);
#2162=VERTEX_POINT('',#6859);
#2163=VERTEX_POINT('',#6861);
#2164=VERTEX_POINT('',#6863);
#2165=VERTEX_POINT('',#6867);
#2166=VERTEX_POINT('',#6869);
#2167=VERTEX_POINT('',#6873);
#2168=VERTEX_POINT('',#6875);
#2169=VERTEX_POINT('',#6885);
#2170=VERTEX_POINT('',#6886);
#2171=VERTEX_POINT('',#6888);
#2172=VERTEX_POINT('',#6890);
#2173=VERTEX_POINT('',#6894);
#2174=VERTEX_POINT('',#6896);
#2175=VERTEX_POINT('',#6900);
#2176=VERTEX_POINT('',#6902);
#2177=VERTEX_POINT('',#6912);
#2178=VERTEX_POINT('',#6913);
#2179=VERTEX_POINT('',#6915);
#2180=VERTEX_POINT('',#6917);
#2181=VERTEX_POINT('',#6921);
#2182=VERTEX_POINT('',#6923);
#2183=VERTEX_POINT('',#6927);
#2184=VERTEX_POINT('',#6929);
#2185=VERTEX_POINT('',#6939);
#2186=VERTEX_POINT('',#6940);
#2187=VERTEX_POINT('',#6944);
#2188=VERTEX_POINT('',#6946);
#2189=VERTEX_POINT('',#6950);
#2190=VERTEX_POINT('',#6951);
#2191=VERTEX_POINT('',#6955);
#2192=VERTEX_POINT('',#6957);
#2193=VERTEX_POINT('',#6961);
#2194=VERTEX_POINT('',#6963);
#2195=VERTEX_POINT('',#6968);
#2196=VERTEX_POINT('',#6970);
#2197=VERTEX_POINT('',#6975);
#2198=VERTEX_POINT('',#6977);
#2199=VERTEX_POINT('',#6981);
#2200=VERTEX_POINT('',#6983);
#2201=VERTEX_POINT('',#6987);
#2202=VERTEX_POINT('',#6988);
#2203=VERTEX_POINT('',#6990);
#2204=VERTEX_POINT('',#6992);
#2205=VERTEX_POINT('',#6996);
#2206=VERTEX_POINT('',#6998);
#2207=VERTEX_POINT('',#7002);
#2208=VERTEX_POINT('',#7004);
#2209=VERTEX_POINT('',#7014);
#2210=VERTEX_POINT('',#7015);
#2211=VERTEX_POINT('',#7019);
#2212=VERTEX_POINT('',#7021);
#2213=VERTEX_POINT('',#7025);
#2214=VERTEX_POINT('',#7026);
#2215=VERTEX_POINT('',#7030);
#2216=VERTEX_POINT('',#7032);
#2217=VERTEX_POINT('',#7036);
#2218=VERTEX_POINT('',#7038);
#2219=VERTEX_POINT('',#7043);
#2220=VERTEX_POINT('',#7045);
#2221=VERTEX_POINT('',#7050);
#2222=VERTEX_POINT('',#7052);
#2223=VERTEX_POINT('',#7056);
#2224=VERTEX_POINT('',#7058);
#2225=VERTEX_POINT('',#7062);
#2226=VERTEX_POINT('',#7063);
#2227=VERTEX_POINT('',#7065);
#2228=VERTEX_POINT('',#7067);
#2229=VERTEX_POINT('',#7071);
#2230=VERTEX_POINT('',#7073);
#2231=VERTEX_POINT('',#7077);
#2232=VERTEX_POINT('',#7079);
#2233=VERTEX_POINT('',#7089);
#2234=VERTEX_POINT('',#7091);
#2235=VERTEX_POINT('',#7095);
#2236=VERTEX_POINT('',#7097);
#2237=VERTEX_POINT('',#7101);
#2238=VERTEX_POINT('',#7103);
#2239=VERTEX_POINT('',#7107);
#2240=VERTEX_POINT('',#7109);
#2241=VERTEX_POINT('',#7113);
#2242=VERTEX_POINT('',#7115);
#2243=VERTEX_POINT('',#7119);
#2244=VERTEX_POINT('',#7121);
#2245=VERTEX_POINT('',#7125);
#2246=VERTEX_POINT('',#7127);
#2247=VERTEX_POINT('',#7131);
#2248=VERTEX_POINT('',#7133);
#2249=VERTEX_POINT('',#7137);
#2250=VERTEX_POINT('',#7139);
#2251=VERTEX_POINT('',#7143);
#2252=VERTEX_POINT('',#7145);
#2253=VERTEX_POINT('',#7149);
#2254=VERTEX_POINT('',#7151);
#2255=VERTEX_POINT('',#7155);
#2256=VERTEX_POINT('',#7157);
#2257=VERTEX_POINT('',#7161);
#2258=VERTEX_POINT('',#7162);
#2259=VERTEX_POINT('',#7164);
#2260=VERTEX_POINT('',#7166);
#2261=VERTEX_POINT('',#7170);
#2262=VERTEX_POINT('',#7172);
#2263=VERTEX_POINT('',#7176);
#2264=VERTEX_POINT('',#7178);
#2265=VERTEX_POINT('',#7188);
#2266=VERTEX_POINT('',#7190);
#2267=VERTEX_POINT('',#7194);
#2268=VERTEX_POINT('',#7196);
#2269=VERTEX_POINT('',#7200);
#2270=VERTEX_POINT('',#7202);
#2271=VERTEX_POINT('',#7206);
#2272=VERTEX_POINT('',#7208);
#2273=VERTEX_POINT('',#7212);
#2274=VERTEX_POINT('',#7214);
#2275=VERTEX_POINT('',#7218);
#2276=VERTEX_POINT('',#7220);
#2277=VERTEX_POINT('',#7224);
#2278=VERTEX_POINT('',#7226);
#2279=VERTEX_POINT('',#7230);
#2280=VERTEX_POINT('',#7232);
#2281=VERTEX_POINT('',#7236);
#2282=VERTEX_POINT('',#7237);
#2283=VERTEX_POINT('',#7239);
#2284=VERTEX_POINT('',#7241);
#2285=VERTEX_POINT('',#7245);
#2286=VERTEX_POINT('',#7247);
#2287=VERTEX_POINT('',#7251);
#2288=VERTEX_POINT('',#7253);
#2289=VERTEX_POINT('',#7260);
#2290=VERTEX_POINT('',#7261);
#2291=VERTEX_POINT('',#7263);
#2292=VERTEX_POINT('',#7265);
#2293=VERTEX_POINT('',#7269);
#2294=VERTEX_POINT('',#7271);
#2295=VERTEX_POINT('',#7275);
#2296=VERTEX_POINT('',#7277);
#2297=VERTEX_POINT('',#7287);
#2298=VERTEX_POINT('',#7289);
#2299=VERTEX_POINT('',#7294);
#2300=VERTEX_POINT('',#7296);
#2301=VERTEX_POINT('',#7301);
#2302=VERTEX_POINT('',#7303);
#2303=VERTEX_POINT('',#7308);
#2304=VERTEX_POINT('',#7310);
#2305=VERTEX_POINT('',#7315);
#2306=VERTEX_POINT('',#7317);
#2307=VERTEX_POINT('',#7322);
#2308=VERTEX_POINT('',#7324);
#2309=VERTEX_POINT('',#7329);
#2310=VERTEX_POINT('',#7331);
#2311=VERTEX_POINT('',#7336);
#2312=VERTEX_POINT('',#7338);
#2313=VERTEX_POINT('',#7343);
#2314=VERTEX_POINT('',#7345);
#2315=VERTEX_POINT('',#7350);
#2316=VERTEX_POINT('',#7352);
#2317=VERTEX_POINT('',#7357);
#2318=VERTEX_POINT('',#7359);
#2319=VERTEX_POINT('',#7363);
#2320=VERTEX_POINT('',#7366);
#2321=VERTEX_POINT('',#7368);
#2322=VERTEX_POINT('',#7372);
#2323=VERTEX_POINT('',#7375);
#2324=VERTEX_POINT('',#7376);
#2325=VERTEX_POINT('',#7387);
#2326=VERTEX_POINT('',#7398);
#2327=VERTEX_POINT('',#7420);
#2328=VERTEX_POINT('',#7422);
#2329=VERTEX_POINT('',#7427);
#2330=VERTEX_POINT('',#7428);
#2331=VERTEX_POINT('',#7439);
#2332=VERTEX_POINT('',#7450);
#2333=VERTEX_POINT('',#7472);
#2334=VERTEX_POINT('',#7474);
#2335=VERTEX_POINT('',#7479);
#2336=VERTEX_POINT('',#7480);
#2337=VERTEX_POINT('',#7491);
#2338=VERTEX_POINT('',#7502);
#2339=VERTEX_POINT('',#7524);
#2340=VERTEX_POINT('',#7526);
#2341=VERTEX_POINT('',#7531);
#2342=VERTEX_POINT('',#7532);
#2343=VERTEX_POINT('',#7543);
#2344=VERTEX_POINT('',#7554);
#2345=VERTEX_POINT('',#7576);
#2346=VERTEX_POINT('',#7578);
#2347=VERTEX_POINT('',#7583);
#2348=VERTEX_POINT('',#7584);
#2349=VERTEX_POINT('',#7586);
#2350=VERTEX_POINT('',#7588);
#2351=VERTEX_POINT('',#7592);
#2352=VERTEX_POINT('',#7594);
#2353=VERTEX_POINT('',#7596);
#2354=VERTEX_POINT('',#7598);
#2355=VERTEX_POINT('',#7602);
#2356=VERTEX_POINT('',#7606);
#2357=VERTEX_POINT('',#7608);
#2358=VERTEX_POINT('',#7613);
#2359=VERTEX_POINT('',#7625);
#2360=VERTEX_POINT('',#7626);
#2361=VERTEX_POINT('',#7628);
#2362=VERTEX_POINT('',#7630);
#2363=VERTEX_POINT('',#7634);
#2364=VERTEX_POINT('',#7636);
#2365=VERTEX_POINT('',#7640);
#2366=VERTEX_POINT('',#7642);
#2367=VERTEX_POINT('',#7652);
#2368=VERTEX_POINT('',#7654);
#2369=VERTEX_POINT('',#7658);
#2370=VERTEX_POINT('',#7660);
#2371=VERTEX_POINT('',#7667);
#2372=VERTEX_POINT('',#7669);
#2373=VERTEX_POINT('',#7673);
#2374=VERTEX_POINT('',#7675);
#2375=VERTEX_POINT('',#7682);
#2376=VERTEX_POINT('',#7684);
#2377=VERTEX_POINT('',#7688);
#2378=VERTEX_POINT('',#7690);
#2379=VERTEX_POINT('',#7697);
#2380=VERTEX_POINT('',#7699);
#2381=VERTEX_POINT('',#7703);
#2382=VERTEX_POINT('',#7705);
#2383=VERTEX_POINT('',#7712);
#2384=VERTEX_POINT('',#7713);
#2385=VERTEX_POINT('',#7715);
#2386=VERTEX_POINT('',#7717);
#2387=VERTEX_POINT('',#7719);
#2388=VERTEX_POINT('',#7721);
#2389=VERTEX_POINT('',#7724);
#2390=VERTEX_POINT('',#7727);
#2391=VERTEX_POINT('',#7729);
#2392=VERTEX_POINT('',#7733);
#2393=VERTEX_POINT('',#7737);
#2394=VERTEX_POINT('',#7741);
#2395=VERTEX_POINT('',#7745);
#2396=VERTEX_POINT('',#7752);
#2397=VERTEX_POINT('',#7758);
#2398=VERTEX_POINT('',#7760);
#2399=VERTEX_POINT('',#7767);
#2400=VERTEX_POINT('',#7769);
#2401=VERTEX_POINT('',#7776);
#2402=VERTEX_POINT('',#7778);
#2403=VERTEX_POINT('',#7782);
#2404=VERTEX_POINT('',#7784);
#2405=VERTEX_POINT('',#7788);
#2406=VERTEX_POINT('',#7789);
#2407=VERTEX_POINT('',#7791);
#2408=VERTEX_POINT('',#7793);
#2409=VERTEX_POINT('',#7797);
#2410=VERTEX_POINT('',#7799);
#2411=VERTEX_POINT('',#7803);
#2412=VERTEX_POINT('',#7805);
#2413=VERTEX_POINT('',#7815);
#2414=VERTEX_POINT('',#7816);
#2415=VERTEX_POINT('',#7818);
#2416=VERTEX_POINT('',#7820);
#2417=VERTEX_POINT('',#7824);
#2418=VERTEX_POINT('',#7826);
#2419=VERTEX_POINT('',#7830);
#2420=VERTEX_POINT('',#7832);
#2421=VERTEX_POINT('',#7836);
#2422=VERTEX_POINT('',#7838);
#2423=VERTEX_POINT('',#7842);
#2424=VERTEX_POINT('',#7844);
#2425=VERTEX_POINT('',#7853);
#2426=VERTEX_POINT('',#7856);
#2427=VERTEX_POINT('',#7859);
#2428=VERTEX_POINT('',#7863);
#2429=VERTEX_POINT('',#7867);
#2430=VERTEX_POINT('',#7871);
#2431=VERTEX_POINT('',#7874);
#2432=VERTEX_POINT('',#7882);
#2433=VERTEX_POINT('',#7884);
#2434=VERTEX_POINT('',#7888);
#2435=VERTEX_POINT('',#7891);
#2436=VERTEX_POINT('',#7892);
#2437=VERTEX_POINT('',#7894);
#2438=VERTEX_POINT('',#7896);
#2439=VERTEX_POINT('',#7898);
#2440=VERTEX_POINT('',#7900);
#2441=VERTEX_POINT('',#7903);
#2442=VERTEX_POINT('',#7906);
#2443=VERTEX_POINT('',#7907);
#2444=VERTEX_POINT('',#7909);
#2445=VERTEX_POINT('',#7911);
#2446=VERTEX_POINT('',#7913);
#2447=VERTEX_POINT('',#7915);
#2448=VERTEX_POINT('',#7918);
#2449=VERTEX_POINT('',#7933);
#2450=VERTEX_POINT('',#7936);
#2451=VERTEX_POINT('',#7940);
#2452=VERTEX_POINT('',#7945);
#2453=VERTEX_POINT('',#7949);
#2454=VERTEX_POINT('',#7955);
#2455=VERTEX_POINT('',#7957);
#2456=VERTEX_POINT('',#7960);
#2457=VERTEX_POINT('',#7964);
#2458=VERTEX_POINT('',#7967);
#2459=VERTEX_POINT('',#7971);
#2460=VERTEX_POINT('',#7979);
#2461=VERTEX_POINT('',#7980);
#2462=VERTEX_POINT('',#7982);
#2463=VERTEX_POINT('',#7984);
#2464=VERTEX_POINT('',#7986);
#2465=VERTEX_POINT('',#7988);
#2466=VERTEX_POINT('',#7991);
#2467=VERTEX_POINT('',#7994);
#2468=VERTEX_POINT('',#7995);
#2469=VERTEX_POINT('',#7997);
#2470=VERTEX_POINT('',#7999);
#2471=VERTEX_POINT('',#8001);
#2472=VERTEX_POINT('',#8003);
#2473=VERTEX_POINT('',#8006);
#2474=VERTEX_POINT('',#8021);
#2475=VERTEX_POINT('',#8025);
#2476=VERTEX_POINT('',#8027);
#2477=VERTEX_POINT('',#8032);
#2478=VERTEX_POINT('',#8036);
#2479=VERTEX_POINT('',#8040);
#2480=VERTEX_POINT('',#8046);
#2481=VERTEX_POINT('',#8049);
#2482=VERTEX_POINT('',#8053);
#2483=VERTEX_POINT('',#8057);
#2484=VERTEX_POINT('',#8061);
#2485=VERTEX_POINT('',#8064);
#2486=VERTEX_POINT('',#8068);
#2487=VERTEX_POINT('',#8072);
#2488=VERTEX_POINT('',#8077);
#2489=VERTEX_POINT('',#8078);
#2490=VERTEX_POINT('',#8080);
#2491=VERTEX_POINT('',#8082);
#2492=VERTEX_POINT('',#8086);
#2493=VERTEX_POINT('',#8088);
#2494=VERTEX_POINT('',#8092);
#2495=VERTEX_POINT('',#8094);
#2496=VERTEX_POINT('',#8098);
#2497=VERTEX_POINT('',#8100);
#2498=VERTEX_POINT('',#8104);
#2499=VERTEX_POINT('',#8106);
#2500=VERTEX_POINT('',#8116);
#2501=VERTEX_POINT('',#8117);
#2502=VERTEX_POINT('',#8119);
#2503=VERTEX_POINT('',#8121);
#2504=VERTEX_POINT('',#8125);
#2505=VERTEX_POINT('',#8127);
#2506=VERTEX_POINT('',#8131);
#2507=VERTEX_POINT('',#8133);
#2508=VERTEX_POINT('',#8137);
#2509=VERTEX_POINT('',#8139);
#2510=VERTEX_POINT('',#8143);
#2511=VERTEX_POINT('',#8145);
#2512=VERTEX_POINT('',#8154);
#2513=VERTEX_POINT('',#8157);
#2514=VERTEX_POINT('',#8160);
#2515=VERTEX_POINT('',#8164);
#2516=VERTEX_POINT('',#8168);
#2517=VERTEX_POINT('',#8172);
#2518=VERTEX_POINT('',#8175);
#2519=EDGE_CURVE('',#2145,#2145,#1945,.T.);
#2520=EDGE_CURVE('',#2145,#2146,#1235,.T.);
#2521=EDGE_CURVE('',#2146,#2146,#1946,.T.);
#2522=EDGE_CURVE('',#2147,#2147,#1947,.T.);
#2523=EDGE_CURVE('',#2147,#2148,#1236,.T.);
#2524=EDGE_CURVE('',#2148,#2148,#1948,.T.);
#2525=EDGE_CURVE('',#2149,#2149,#1949,.T.);
#2526=EDGE_CURVE('',#2149,#2150,#1237,.T.);
#2527=EDGE_CURVE('',#2150,#2150,#1950,.T.);
#2528=EDGE_CURVE('',#2151,#2151,#1951,.T.);
#2529=EDGE_CURVE('',#2151,#2152,#1238,.T.);
#2530=EDGE_CURVE('',#2152,#2152,#1952,.T.);
#2531=EDGE_CURVE('',#2153,#2153,#1953,.T.);
#2532=EDGE_CURVE('',#2153,#2154,#1239,.T.);
#2533=EDGE_CURVE('',#2154,#2154,#1954,.T.);
#2534=EDGE_CURVE('',#2155,#2155,#1955,.T.);
#2535=EDGE_CURVE('',#2155,#2156,#1240,.T.);
#2536=EDGE_CURVE('',#2156,#2156,#1956,.T.);
#2537=EDGE_CURVE('',#2157,#2157,#1957,.T.);
#2538=EDGE_CURVE('',#2157,#2158,#1241,.T.);
#2539=EDGE_CURVE('',#2158,#2158,#1958,.T.);
#2540=EDGE_CURVE('',#2159,#2159,#1959,.T.);
#2541=EDGE_CURVE('',#2159,#2160,#1242,.T.);
#2542=EDGE_CURVE('',#2160,#2160,#1960,.T.);
#2543=EDGE_CURVE('',#2161,#2162,#1243,.T.);
#2544=EDGE_CURVE('',#2162,#2163,#1244,.T.);
#2545=EDGE_CURVE('',#2164,#2163,#1245,.T.);
#2546=EDGE_CURVE('',#2161,#2164,#1246,.T.);
#2547=EDGE_CURVE('',#2165,#2161,#1247,.T.);
#2548=EDGE_CURVE('',#2166,#2164,#1248,.T.);
#2549=EDGE_CURVE('',#2165,#2166,#1249,.T.);
#2550=EDGE_CURVE('',#2167,#2165,#1250,.T.);
#2551=EDGE_CURVE('',#2168,#2166,#1251,.T.);
#2552=EDGE_CURVE('',#2167,#2168,#1252,.T.);
#2553=EDGE_CURVE('',#2162,#2167,#1253,.T.);
#2554=EDGE_CURVE('',#2163,#2168,#1254,.T.);
#2555=EDGE_CURVE('',#2169,#2170,#1255,.T.);
#2556=EDGE_CURVE('',#2170,#2171,#1256,.T.);
#2557=EDGE_CURVE('',#2172,#2171,#1257,.T.);
#2558=EDGE_CURVE('',#2169,#2172,#1258,.T.);
#2559=EDGE_CURVE('',#2173,#2169,#1259,.T.);
#2560=EDGE_CURVE('',#2174,#2172,#1260,.T.);
#2561=EDGE_CURVE('',#2173,#2174,#1261,.T.);
#2562=EDGE_CURVE('',#2175,#2173,#1262,.T.);
#2563=EDGE_CURVE('',#2176,#2174,#1263,.T.);
#2564=EDGE_CURVE('',#2175,#2176,#1264,.T.);
#2565=EDGE_CURVE('',#2170,#2175,#1265,.T.);
#2566=EDGE_CURVE('',#2171,#2176,#1266,.T.);
#2567=EDGE_CURVE('',#2177,#2178,#1267,.T.);
#2568=EDGE_CURVE('',#2178,#2179,#1268,.T.);
#2569=EDGE_CURVE('',#2180,#2179,#1269,.T.);
#2570=EDGE_CURVE('',#2177,#2180,#1270,.T.);
#2571=EDGE_CURVE('',#2181,#2177,#1271,.T.);
#2572=EDGE_CURVE('',#2182,#2180,#1272,.T.);
#2573=EDGE_CURVE('',#2181,#2182,#1273,.T.);
#2574=EDGE_CURVE('',#2183,#2181,#1274,.T.);
#2575=EDGE_CURVE('',#2184,#2182,#1275,.T.);
#2576=EDGE_CURVE('',#2183,#2184,#1276,.T.);
#2577=EDGE_CURVE('',#2178,#2183,#1277,.T.);
#2578=EDGE_CURVE('',#2179,#2184,#1278,.T.);
#2579=EDGE_CURVE('',#2185,#2186,#1961,.T.);
#2580=EDGE_CURVE('',#2185,#2186,#1962,.T.);
#2581=EDGE_CURVE('',#2187,#2185,#1279,.T.);
#2582=EDGE_CURVE('',#2188,#2187,#1963,.T.);
#2583=EDGE_CURVE('',#2186,#2188,#1280,.T.);
#2584=EDGE_CURVE('',#2189,#2190,#1964,.T.);
#2585=EDGE_CURVE('',#2189,#2190,#1965,.T.);
#2586=EDGE_CURVE('',#2191,#2189,#1281,.T.);
#2587=EDGE_CURVE('',#2192,#2191,#1966,.T.);
#2588=EDGE_CURVE('',#2190,#2192,#1282,.T.);
#2589=EDGE_CURVE('',#2193,#2193,#1967,.T.);
#2590=EDGE_CURVE('',#2193,#2194,#1283,.T.);
#2591=EDGE_CURVE('',#2187,#2194,#1968,.T.);
#2592=EDGE_CURVE('',#2194,#2188,#1969,.T.);
#2593=EDGE_CURVE('',#2195,#2195,#1970,.T.);
#2594=EDGE_CURVE('',#2195,#2196,#1284,.T.);
#2595=EDGE_CURVE('',#2191,#2196,#1971,.T.);
#2596=EDGE_CURVE('',#2196,#2192,#1972,.T.);
#2597=EDGE_CURVE('',#2197,#2197,#1973,.T.);
#2598=EDGE_CURVE('',#2197,#2198,#1285,.T.);
#2599=EDGE_CURVE('',#2198,#2198,#1974,.T.);
#2600=EDGE_CURVE('',#2199,#2199,#1975,.T.);
#2601=EDGE_CURVE('',#2199,#2200,#1286,.T.);
#2602=EDGE_CURVE('',#2200,#2200,#1976,.T.);
#2603=EDGE_CURVE('',#2201,#2202,#1287,.T.);
#2604=EDGE_CURVE('',#2202,#2203,#1288,.T.);
#2605=EDGE_CURVE('',#2204,#2203,#1289,.T.);
#2606=EDGE_CURVE('',#2201,#2204,#1290,.T.);
#2607=EDGE_CURVE('',#2205,#2201,#1291,.T.);
#2608=EDGE_CURVE('',#2206,#2204,#1292,.T.);
#2609=EDGE_CURVE('',#2205,#2206,#1293,.T.);
#2610=EDGE_CURVE('',#2207,#2205,#1294,.T.);
#2611=EDGE_CURVE('',#2208,#2206,#1295,.T.);
#2612=EDGE_CURVE('',#2207,#2208,#1296,.T.);
#2613=EDGE_CURVE('',#2202,#2207,#1297,.T.);
#2614=EDGE_CURVE('',#2203,#2208,#1298,.T.);
#2615=EDGE_CURVE('',#2209,#2210,#1977,.T.);
#2616=EDGE_CURVE('',#2209,#2210,#1978,.T.);
#2617=EDGE_CURVE('',#2211,#2209,#1299,.T.);
#2618=EDGE_CURVE('',#2212,#2211,#1979,.T.);
#2619=EDGE_CURVE('',#2210,#2212,#1300,.T.);
#2620=EDGE_CURVE('',#2213,#2214,#1980,.T.);
#2621=EDGE_CURVE('',#2213,#2214,#1981,.T.);
#2622=EDGE_CURVE('',#2215,#2213,#1301,.T.);
#2623=EDGE_CURVE('',#2216,#2215,#1982,.T.);
#2624=EDGE_CURVE('',#2214,#2216,#1302,.T.);
#2625=EDGE_CURVE('',#2217,#2217,#1983,.T.);
#2626=EDGE_CURVE('',#2217,#2218,#1303,.T.);
#2627=EDGE_CURVE('',#2211,#2218,#1984,.T.);
#2628=EDGE_CURVE('',#2218,#2212,#1985,.T.);
#2629=EDGE_CURVE('',#2219,#2219,#1986,.T.);
#2630=EDGE_CURVE('',#2219,#2220,#1304,.T.);
#2631=EDGE_CURVE('',#2215,#2220,#1987,.T.);
#2632=EDGE_CURVE('',#2220,#2216,#1988,.T.);
#2633=EDGE_CURVE('',#2221,#2221,#1989,.T.);
#2634=EDGE_CURVE('',#2221,#2222,#1305,.T.);
#2635=EDGE_CURVE('',#2222,#2222,#1990,.T.);
#2636=EDGE_CURVE('',#2223,#2223,#1991,.T.);
#2637=EDGE_CURVE('',#2223,#2224,#1306,.T.);
#2638=EDGE_CURVE('',#2224,#2224,#1992,.T.);
#2639=EDGE_CURVE('',#2225,#2226,#1307,.T.);
#2640=EDGE_CURVE('',#2226,#2227,#1308,.T.);
#2641=EDGE_CURVE('',#2228,#2227,#1309,.T.);
#2642=EDGE_CURVE('',#2225,#2228,#1310,.T.);
#2643=EDGE_CURVE('',#2229,#2225,#1311,.T.);
#2644=EDGE_CURVE('',#2230,#2228,#1312,.T.);
#2645=EDGE_CURVE('',#2229,#2230,#1313,.T.);
#2646=EDGE_CURVE('',#2231,#2229,#1314,.T.);
#2647=EDGE_CURVE('',#2232,#2230,#1315,.T.);
#2648=EDGE_CURVE('',#2231,#2232,#1316,.T.);
#2649=EDGE_CURVE('',#2226,#2231,#1317,.T.);
#2650=EDGE_CURVE('',#2227,#2232,#1318,.T.);
#2651=EDGE_CURVE('',#2233,#2233,#1993,.T.);
#2652=EDGE_CURVE('',#2233,#2234,#1319,.T.);
#2653=EDGE_CURVE('',#2234,#2234,#1994,.T.);
#2654=EDGE_CURVE('',#2235,#2235,#1995,.T.);
#2655=EDGE_CURVE('',#2235,#2236,#1320,.T.);
#2656=EDGE_CURVE('',#2236,#2236,#1996,.T.);
#2657=EDGE_CURVE('',#2237,#2237,#1997,.T.);
#2658=EDGE_CURVE('',#2237,#2238,#1321,.T.);
#2659=EDGE_CURVE('',#2238,#2238,#1998,.T.);
#2660=EDGE_CURVE('',#2239,#2239,#1999,.T.);
#2661=EDGE_CURVE('',#2239,#2240,#1322,.T.);
#2662=EDGE_CURVE('',#2240,#2240,#2000,.T.);
#2663=EDGE_CURVE('',#2241,#2241,#2001,.T.);
#2664=EDGE_CURVE('',#2241,#2242,#1323,.T.);
#2665=EDGE_CURVE('',#2242,#2242,#2002,.T.);
#2666=EDGE_CURVE('',#2243,#2243,#2003,.T.);
#2667=EDGE_CURVE('',#2243,#2244,#1324,.T.);
#2668=EDGE_CURVE('',#2244,#2244,#2004,.T.);
#2669=EDGE_CURVE('',#2245,#2245,#2005,.T.);
#2670=EDGE_CURVE('',#2245,#2246,#1325,.T.);
#2671=EDGE_CURVE('',#2246,#2246,#2006,.T.);
#2672=EDGE_CURVE('',#2247,#2247,#2007,.T.);
#2673=EDGE_CURVE('',#2247,#2248,#1326,.T.);
#2674=EDGE_CURVE('',#2248,#2248,#2008,.T.);
#2675=EDGE_CURVE('',#2249,#2249,#2009,.T.);
#2676=EDGE_CURVE('',#2249,#2250,#1327,.T.);
#2677=EDGE_CURVE('',#2250,#2250,#2010,.T.);
#2678=EDGE_CURVE('',#2251,#2251,#2011,.T.);
#2679=EDGE_CURVE('',#2251,#2252,#1328,.T.);
#2680=EDGE_CURVE('',#2252,#2252,#2012,.T.);
#2681=EDGE_CURVE('',#2253,#2253,#2013,.T.);
#2682=EDGE_CURVE('',#2253,#2254,#1329,.T.);
#2683=EDGE_CURVE('',#2254,#2254,#2014,.T.);
#2684=EDGE_CURVE('',#2255,#2255,#2015,.T.);
#2685=EDGE_CURVE('',#2255,#2256,#1330,.T.);
#2686=EDGE_CURVE('',#2256,#2256,#2016,.T.);
#2687=EDGE_CURVE('',#2257,#2258,#1331,.T.);
#2688=EDGE_CURVE('',#2258,#2259,#1332,.T.);
#2689=EDGE_CURVE('',#2260,#2259,#1333,.T.);
#2690=EDGE_CURVE('',#2257,#2260,#1334,.T.);
#2691=EDGE_CURVE('',#2261,#2257,#1335,.T.);
#2692=EDGE_CURVE('',#2262,#2260,#1336,.T.);
#2693=EDGE_CURVE('',#2261,#2262,#1337,.T.);
#2694=EDGE_CURVE('',#2263,#2261,#1338,.T.);
#2695=EDGE_CURVE('',#2264,#2262,#1339,.T.);
#2696=EDGE_CURVE('',#2263,#2264,#1340,.T.);
#2697=EDGE_CURVE('',#2258,#2263,#1341,.T.);
#2698=EDGE_CURVE('',#2259,#2264,#1342,.T.);
#2699=EDGE_CURVE('',#2265,#2265,#2017,.T.);
#2700=EDGE_CURVE('',#2265,#2266,#1343,.T.);
#2701=EDGE_CURVE('',#2266,#2266,#2018,.T.);
#2702=EDGE_CURVE('',#2267,#2267,#2019,.T.);
#2703=EDGE_CURVE('',#2267,#2268,#1344,.T.);
#2704=EDGE_CURVE('',#2268,#2268,#2020,.T.);
#2705=EDGE_CURVE('',#2269,#2269,#2021,.T.);
#2706=EDGE_CURVE('',#2269,#2270,#1345,.T.);
#2707=EDGE_CURVE('',#2270,#2270,#2022,.T.);
#2708=EDGE_CURVE('',#2271,#2271,#2023,.T.);
#2709=EDGE_CURVE('',#2271,#2272,#1346,.T.);
#2710=EDGE_CURVE('',#2272,#2272,#2024,.T.);
#2711=EDGE_CURVE('',#2273,#2273,#2025,.T.);
#2712=EDGE_CURVE('',#2273,#2274,#1347,.T.);
#2713=EDGE_CURVE('',#2274,#2274,#2026,.T.);
#2714=EDGE_CURVE('',#2275,#2275,#2027,.T.);
#2715=EDGE_CURVE('',#2275,#2276,#1348,.T.);
#2716=EDGE_CURVE('',#2276,#2276,#2028,.T.);
#2717=EDGE_CURVE('',#2277,#2277,#2029,.T.);
#2718=EDGE_CURVE('',#2277,#2278,#1349,.T.);
#2719=EDGE_CURVE('',#2278,#2278,#2030,.T.);
#2720=EDGE_CURVE('',#2279,#2279,#2031,.T.);
#2721=EDGE_CURVE('',#2279,#2280,#1350,.T.);
#2722=EDGE_CURVE('',#2280,#2280,#2032,.T.);
#2723=EDGE_CURVE('',#2281,#2282,#1351,.T.);
#2724=EDGE_CURVE('',#2283,#2281,#1352,.T.);
#2725=EDGE_CURVE('',#2284,#2283,#1353,.T.);
#2726=EDGE_CURVE('',#2284,#2282,#1354,.T.);
#2727=EDGE_CURVE('',#2282,#2285,#1355,.T.);
#2728=EDGE_CURVE('',#2286,#2284,#1356,.T.);
#2729=EDGE_CURVE('',#2286,#2285,#1357,.T.);
#2730=EDGE_CURVE('',#2285,#2287,#1358,.T.);
#2731=EDGE_CURVE('',#2288,#2286,#1359,.T.);
#2732=EDGE_CURVE('',#2288,#2287,#1360,.T.);
#2733=EDGE_CURVE('',#2287,#2281,#1361,.T.);
#2734=EDGE_CURVE('',#2283,#2288,#1362,.T.);
#2735=EDGE_CURVE('',#2289,#2290,#1363,.T.);
#2736=EDGE_CURVE('',#2290,#2291,#1364,.T.);
#2737=EDGE_CURVE('',#2292,#2291,#1365,.T.);
#2738=EDGE_CURVE('',#2289,#2292,#1366,.T.);
#2739=EDGE_CURVE('',#2293,#2289,#1367,.T.);
#2740=EDGE_CURVE('',#2294,#2292,#1368,.T.);
#2741=EDGE_CURVE('',#2293,#2294,#1369,.T.);
#2742=EDGE_CURVE('',#2295,#2293,#1370,.T.);
#2743=EDGE_CURVE('',#2296,#2294,#1371,.T.);
#2744=EDGE_CURVE('',#2295,#2296,#1372,.T.);
#2745=EDGE_CURVE('',#2290,#2295,#1373,.T.);
#2746=EDGE_CURVE('',#2291,#2296,#1374,.T.);
#2747=EDGE_CURVE('',#2297,#2297,#2033,.T.);
#2748=EDGE_CURVE('',#2297,#2298,#1375,.T.);
#2749=EDGE_CURVE('',#2298,#2298,#2034,.T.);
#2750=EDGE_CURVE('',#2299,#2299,#2035,.T.);
#2751=EDGE_CURVE('',#2299,#2300,#1376,.T.);
#2752=EDGE_CURVE('',#2300,#2300,#2036,.T.);
#2753=EDGE_CURVE('',#2301,#2301,#2037,.T.);
#2754=EDGE_CURVE('',#2301,#2302,#1377,.T.);
#2755=EDGE_CURVE('',#2302,#2302,#2038,.T.);
#2756=EDGE_CURVE('',#2303,#2303,#2039,.T.);
#2757=EDGE_CURVE('',#2303,#2304,#1378,.T.);
#2758=EDGE_CURVE('',#2304,#2304,#2040,.T.);
#2759=EDGE_CURVE('',#2305,#2305,#2041,.T.);
#2760=EDGE_CURVE('',#2305,#2306,#1379,.T.);
#2761=EDGE_CURVE('',#2306,#2306,#2042,.T.);
#2762=EDGE_CURVE('',#2307,#2307,#2043,.T.);
#2763=EDGE_CURVE('',#2307,#2308,#1380,.T.);
#2764=EDGE_CURVE('',#2308,#2308,#2044,.T.);
#2765=EDGE_CURVE('',#2309,#2309,#2045,.T.);
#2766=EDGE_CURVE('',#2309,#2310,#1381,.T.);
#2767=EDGE_CURVE('',#2310,#2310,#2046,.T.);
#2768=EDGE_CURVE('',#2311,#2311,#2047,.T.);
#2769=EDGE_CURVE('',#2311,#2312,#1382,.T.);
#2770=EDGE_CURVE('',#2312,#2312,#2048,.T.);
#2771=EDGE_CURVE('',#2313,#2313,#2049,.T.);
#2772=EDGE_CURVE('',#2313,#2314,#1383,.T.);
#2773=EDGE_CURVE('',#2314,#2314,#2050,.T.);
#2774=EDGE_CURVE('',#2315,#2315,#2051,.T.);
#2775=EDGE_CURVE('',#2315,#2316,#1384,.T.);
#2776=EDGE_CURVE('',#2316,#2316,#2052,.T.);
#2777=EDGE_CURVE('',#2317,#2317,#2053,.T.);
#2778=EDGE_CURVE('',#2317,#2318,#1385,.T.);
#2779=EDGE_CURVE('',#2318,#2318,#2054,.T.);
#2780=EDGE_CURVE('',#2319,#2319,#2055,.T.);
#2781=EDGE_CURVE('',#2320,#2320,#2056,.T.);
#2782=EDGE_CURVE('',#2320,#2321,#1386,.T.);
#2783=EDGE_CURVE('',#2321,#2321,#2057,.T.);
#2784=EDGE_CURVE('',#2322,#2322,#2058,.T.);
#2785=EDGE_CURVE('',#2323,#2324,#185,.T.);
#2786=EDGE_CURVE('',#2325,#2323,#186,.T.);
#2787=EDGE_CURVE('',#2325,#2326,#1387,.T.);
#2788=EDGE_CURVE('',#2326,#2326,#2059,.T.);
#2789=EDGE_CURVE('',#2324,#2325,#187,.T.);
#2790=EDGE_CURVE('',#2327,#2327,#2060,.T.);
#2791=EDGE_CURVE('',#2327,#2328,#1388,.T.);
#2792=EDGE_CURVE('',#2328,#2328,#2061,.T.);
#2793=EDGE_CURVE('',#2329,#2330,#188,.T.);
#2794=EDGE_CURVE('',#2331,#2329,#189,.T.);
#2795=EDGE_CURVE('',#2331,#2332,#1389,.T.);
#2796=EDGE_CURVE('',#2332,#2332,#2062,.T.);
#2797=EDGE_CURVE('',#2330,#2331,#190,.T.);
#2798=EDGE_CURVE('',#2333,#2333,#2063,.T.);
#2799=EDGE_CURVE('',#2333,#2334,#1390,.T.);
#2800=EDGE_CURVE('',#2334,#2334,#2064,.T.);
#2801=EDGE_CURVE('',#2335,#2336,#191,.T.);
#2802=EDGE_CURVE('',#2337,#2335,#192,.T.);
#2803=EDGE_CURVE('',#2337,#2338,#1391,.T.);
#2804=EDGE_CURVE('',#2338,#2338,#2065,.T.);
#2805=EDGE_CURVE('',#2336,#2337,#193,.T.);
#2806=EDGE_CURVE('',#2339,#2339,#2066,.T.);
#2807=EDGE_CURVE('',#2339,#2340,#1392,.T.);
#2808=EDGE_CURVE('',#2340,#2340,#2067,.T.);
#2809=EDGE_CURVE('',#2341,#2342,#194,.T.);
#2810=EDGE_CURVE('',#2343,#2341,#195,.T.);
#2811=EDGE_CURVE('',#2343,#2344,#1393,.T.);
#2812=EDGE_CURVE('',#2344,#2344,#2068,.T.);
#2813=EDGE_CURVE('',#2342,#2343,#196,.T.);
#2814=EDGE_CURVE('',#2345,#2345,#2069,.T.);
#2815=EDGE_CURVE('',#2345,#2346,#1394,.T.);
#2816=EDGE_CURVE('',#2346,#2346,#2070,.T.);
#2817=EDGE_CURVE('',#2347,#2348,#1395,.T.);
#2818=EDGE_CURVE('',#2347,#2349,#1396,.T.);
#2819=EDGE_CURVE('',#2349,#2350,#1397,.T.);
#2820=EDGE_CURVE('',#2348,#2350,#1398,.T.);
#2821=EDGE_CURVE('',#2348,#2351,#1399,.T.);
#2822=EDGE_CURVE('',#2350,#2352,#1400,.T.);
#2823=EDGE_CURVE('',#2353,#2352,#2071,.T.);
#2824=EDGE_CURVE('',#2353,#2354,#1401,.T.);
#2825=EDGE_CURVE('',#2351,#2354,#1402,.T.);
#2826=EDGE_CURVE('',#2352,#2355,#1403,.T.);
#2827=EDGE_CURVE('',#2355,#2349,#1404,.T.);
#2828=EDGE_CURVE('',#2351,#2356,#1405,.T.);
#2829=EDGE_CURVE('',#2354,#2357,#1406,.T.);
#2830=EDGE_CURVE('',#2356,#2357,#1407,.T.);
#2831=EDGE_CURVE('',#2356,#2347,#1408,.T.);
#2832=EDGE_CURVE('',#2357,#2358,#1409,.T.);
#2833=EDGE_CURVE('',#2355,#2358,#2072,.T.);
#2834=EDGE_CURVE('',#2358,#2353,#1410,.T.);
#2835=EDGE_CURVE('',#2322,#2343,#1411,.T.);
#2836=EDGE_CURVE('',#2342,#2337,#1412,.T.);
#2837=EDGE_CURVE('',#2336,#2331,#1413,.T.);
#2838=EDGE_CURVE('',#2330,#2325,#1414,.T.);
#2839=EDGE_CURVE('',#2324,#2319,#1415,.T.);
#2840=EDGE_CURVE('',#2359,#2360,#1416,.T.);
#2841=EDGE_CURVE('',#2360,#2361,#1417,.T.);
#2842=EDGE_CURVE('',#2362,#2361,#1418,.T.);
#2843=EDGE_CURVE('',#2359,#2362,#1419,.T.);
#2844=EDGE_CURVE('',#2363,#2359,#1420,.T.);
#2845=EDGE_CURVE('',#2364,#2362,#1421,.T.);
#2846=EDGE_CURVE('',#2363,#2364,#1422,.T.);
#2847=EDGE_CURVE('',#2365,#2363,#1423,.T.);
#2848=EDGE_CURVE('',#2366,#2364,#1424,.T.);
#2849=EDGE_CURVE('',#2365,#2366,#1425,.T.);
#2850=EDGE_CURVE('',#2360,#2365,#1426,.T.);
#2851=EDGE_CURVE('',#2361,#2366,#1427,.T.);
#2852=EDGE_CURVE('',#2367,#2367,#2073,.T.);
#2853=EDGE_CURVE('',#2367,#2368,#1428,.T.);
#2854=EDGE_CURVE('',#2368,#2368,#2074,.T.);
#2855=EDGE_CURVE('',#2369,#2369,#2075,.T.);
#2856=EDGE_CURVE('',#2369,#2370,#1429,.T.);
#2857=EDGE_CURVE('',#2370,#2370,#2076,.T.);
#2858=EDGE_CURVE('',#2371,#2371,#2077,.T.);
#2859=EDGE_CURVE('',#2371,#2372,#1430,.T.);
#2860=EDGE_CURVE('',#2372,#2372,#2078,.T.);
#2861=EDGE_CURVE('',#2373,#2373,#2079,.T.);
#2862=EDGE_CURVE('',#2373,#2374,#1431,.T.);
#2863=EDGE_CURVE('',#2374,#2374,#2080,.T.);
#2864=EDGE_CURVE('',#2375,#2375,#2081,.T.);
#2865=EDGE_CURVE('',#2375,#2376,#1432,.T.);
#2866=EDGE_CURVE('',#2376,#2376,#2082,.T.);
#2867=EDGE_CURVE('',#2377,#2377,#2083,.T.);
#2868=EDGE_CURVE('',#2377,#2378,#1433,.T.);
#2869=EDGE_CURVE('',#2378,#2378,#2084,.T.);
#2870=EDGE_CURVE('',#2379,#2379,#2085,.T.);
#2871=EDGE_CURVE('',#2379,#2380,#1434,.T.);
#2872=EDGE_CURVE('',#2380,#2380,#2086,.T.);
#2873=EDGE_CURVE('',#2381,#2381,#2087,.T.);
#2874=EDGE_CURVE('',#2381,#2382,#1435,.T.);
#2875=EDGE_CURVE('',#2382,#2382,#2088,.T.);
#2876=EDGE_CURVE('',#2383,#2384,#1436,.T.);
#2877=EDGE_CURVE('',#2385,#2383,#1437,.T.);
#2878=EDGE_CURVE('',#2386,#2385,#1438,.T.);
#2879=EDGE_CURVE('',#2387,#2386,#1439,.T.);
#2880=EDGE_CURVE('',#2388,#2387,#1440,.T.);
#2881=EDGE_CURVE('',#2384,#2388,#1441,.T.);
#2882=EDGE_CURVE('',#2389,#2389,#2089,.T.);
#2883=EDGE_CURVE('',#2383,#2390,#1442,.T.);
#2884=EDGE_CURVE('',#2391,#2390,#1443,.T.);
#2885=EDGE_CURVE('',#2385,#2391,#1444,.T.);
#2886=EDGE_CURVE('',#2392,#2391,#1445,.T.);
#2887=EDGE_CURVE('',#2386,#2392,#1446,.T.);
#2888=EDGE_CURVE('',#2393,#2392,#1447,.T.);
#2889=EDGE_CURVE('',#2387,#2393,#1448,.T.);
#2890=EDGE_CURVE('',#2394,#2393,#1449,.T.);
#2891=EDGE_CURVE('',#2388,#2394,#1450,.T.);
#2892=EDGE_CURVE('',#2395,#2394,#1451,.T.);
#2893=EDGE_CURVE('',#2384,#2395,#1452,.T.);
#2894=EDGE_CURVE('',#2390,#2395,#1453,.T.);
#2895=EDGE_CURVE('',#2389,#2396,#1454,.T.);
#2896=EDGE_CURVE('',#2396,#2396,#2090,.T.);
#2897=EDGE_CURVE('',#2397,#2397,#2091,.T.);
#2898=EDGE_CURVE('',#2397,#2398,#1455,.T.);
#2899=EDGE_CURVE('',#2398,#2398,#2092,.T.);
#2900=EDGE_CURVE('',#2399,#2399,#2093,.T.);
#2901=EDGE_CURVE('',#2399,#2400,#1456,.T.);
#2902=EDGE_CURVE('',#2400,#2400,#2094,.T.);
#2903=EDGE_CURVE('',#2401,#2401,#2095,.T.);
#2904=EDGE_CURVE('',#2401,#2402,#1457,.T.);
#2905=EDGE_CURVE('',#2402,#2402,#2096,.T.);
#2906=EDGE_CURVE('',#2403,#2403,#2097,.T.);
#2907=EDGE_CURVE('',#2403,#2404,#1458,.T.);
#2908=EDGE_CURVE('',#2404,#2404,#2098,.T.);
#2909=EDGE_CURVE('',#2405,#2406,#1459,.T.);
#2910=EDGE_CURVE('',#2406,#2407,#1460,.T.);
#2911=EDGE_CURVE('',#2408,#2407,#1461,.T.);
#2912=EDGE_CURVE('',#2405,#2408,#1462,.T.);
#2913=EDGE_CURVE('',#2409,#2405,#1463,.T.);
#2914=EDGE_CURVE('',#2410,#2408,#1464,.T.);
#2915=EDGE_CURVE('',#2409,#2410,#1465,.T.);
#2916=EDGE_CURVE('',#2411,#2409,#1466,.T.);
#2917=EDGE_CURVE('',#2412,#2410,#1467,.T.);
#2918=EDGE_CURVE('',#2411,#2412,#1468,.T.);
#2919=EDGE_CURVE('',#2406,#2411,#1469,.T.);
#2920=EDGE_CURVE('',#2407,#2412,#1470,.T.);
#2921=EDGE_CURVE('',#2413,#2414,#1471,.T.);
#2922=EDGE_CURVE('',#2414,#2415,#1472,.T.);
#2923=EDGE_CURVE('',#2415,#2416,#1473,.T.);
#2924=EDGE_CURVE('',#2413,#2416,#1474,.T.);
#2925=EDGE_CURVE('',#2414,#2417,#1475,.T.);
#2926=EDGE_CURVE('',#2417,#2418,#1476,.T.);
#2927=EDGE_CURVE('',#2418,#2415,#1477,.T.);
#2928=EDGE_CURVE('',#2417,#2419,#1478,.T.);
#2929=EDGE_CURVE('',#2419,#2420,#1479,.T.);
#2930=EDGE_CURVE('',#2420,#2418,#1480,.T.);
#2931=EDGE_CURVE('',#2419,#2421,#1481,.T.);
#2932=EDGE_CURVE('',#2421,#2422,#1482,.T.);
#2933=EDGE_CURVE('',#2422,#2420,#1483,.T.);
#2934=EDGE_CURVE('',#2421,#2423,#1484,.T.);
#2935=EDGE_CURVE('',#2423,#2424,#1485,.T.);
#2936=EDGE_CURVE('',#2424,#2422,#1486,.T.);
#2937=EDGE_CURVE('',#2423,#2413,#1487,.T.);
#2938=EDGE_CURVE('',#2416,#2424,#1488,.T.);
#2939=EDGE_CURVE('',#2425,#2425,#2099,.T.);
#2940=EDGE_CURVE('',#2426,#2426,#2100,.T.);
#2941=EDGE_CURVE('',#2427,#2427,#2101,.T.);
#2942=EDGE_CURVE('',#2427,#2426,#1489,.T.);
#2943=EDGE_CURVE('',#2428,#2428,#2102,.T.);
#2944=EDGE_CURVE('',#2428,#2427,#1490,.T.);
#2945=EDGE_CURVE('',#2429,#2429,#2103,.T.);
#2946=EDGE_CURVE('',#2429,#2428,#1491,.T.);
#2947=EDGE_CURVE('',#2430,#2430,#2104,.T.);
#2948=EDGE_CURVE('',#2431,#2431,#2105,.F.);
#2949=EDGE_CURVE('',#2431,#2430,#1492,.T.);
#2950=EDGE_CURVE('',#2425,#2431,#1493,.T.);
#2951=EDGE_CURVE('',#2432,#2432,#2106,.T.);
#2952=EDGE_CURVE('',#2432,#2433,#1494,.T.);
#2953=EDGE_CURVE('',#2433,#2433,#2107,.T.);
#2954=EDGE_CURVE('',#2434,#2434,#2108,.T.);
#2955=EDGE_CURVE('',#2435,#2436,#1495,.T.);
#2956=EDGE_CURVE('',#2436,#2437,#1496,.T.);
#2957=EDGE_CURVE('',#2437,#2438,#1497,.T.);
#2958=EDGE_CURVE('',#2438,#2439,#1498,.T.);
#2959=EDGE_CURVE('',#2439,#2440,#1499,.T.);
#2960=EDGE_CURVE('',#2440,#2435,#1500,.T.);
#2961=EDGE_CURVE('',#2441,#2441,#2109,.T.);
#2962=EDGE_CURVE('',#2442,#2443,#1501,.T.);
#2963=EDGE_CURVE('',#2444,#2442,#1502,.T.);
#2964=EDGE_CURVE('',#2445,#2444,#1503,.T.);
#2965=EDGE_CURVE('',#2446,#2445,#1504,.T.);
#2966=EDGE_CURVE('',#2447,#2446,#1505,.T.);
#2967=EDGE_CURVE('',#2443,#2447,#1506,.T.);
#2968=EDGE_CURVE('',#2448,#2448,#2110,.T.);
#2969=EDGE_CURVE('',#2442,#2435,#1507,.T.);
#2970=EDGE_CURVE('',#2444,#2440,#1508,.T.);
#2971=EDGE_CURVE('',#2445,#2439,#1509,.T.);
#2972=EDGE_CURVE('',#2446,#2438,#1510,.T.);
#2973=EDGE_CURVE('',#2447,#2437,#1511,.T.);
#2974=EDGE_CURVE('',#2443,#2436,#1512,.T.);
#2975=EDGE_CURVE('',#2449,#2449,#2111,.T.);
#2976=EDGE_CURVE('',#2449,#2450,#1513,.T.);
#2977=EDGE_CURVE('',#2450,#2450,#2112,.T.);
#2978=EDGE_CURVE('',#2451,#2451,#2113,.T.);
#2979=EDGE_CURVE('',#2441,#2451,#1514,.T.);
#2980=EDGE_CURVE('',#2452,#2452,#2114,.T.);
#2981=EDGE_CURVE('',#2452,#2448,#1515,.T.);
#2982=EDGE_CURVE('',#2453,#2453,#2115,.T.);
#2983=EDGE_CURVE('',#2453,#2434,#1516,.T.);
#2984=EDGE_CURVE('',#2454,#2454,#2116,.T.);
#2985=EDGE_CURVE('',#2455,#2455,#2117,.T.);
#2986=EDGE_CURVE('',#2456,#2456,#2118,.T.);
#2987=EDGE_CURVE('',#2456,#2454,#1517,.T.);
#2988=EDGE_CURVE('',#2457,#2457,#2119,.T.);
#2989=EDGE_CURVE('',#2458,#2458,#2120,.T.);
#2990=EDGE_CURVE('',#2458,#2457,#1518,.T.);
#2991=EDGE_CURVE('',#2459,#2459,#2121,.T.);
#2992=EDGE_CURVE('',#2459,#2455,#1519,.T.);
#2993=EDGE_CURVE('',#2460,#2461,#1520,.T.);
#2994=EDGE_CURVE('',#2461,#2462,#1521,.T.);
#2995=EDGE_CURVE('',#2462,#2463,#1522,.T.);
#2996=EDGE_CURVE('',#2463,#2464,#1523,.T.);
#2997=EDGE_CURVE('',#2464,#2465,#1524,.T.);
#2998=EDGE_CURVE('',#2465,#2460,#1525,.T.);
#2999=EDGE_CURVE('',#2466,#2466,#2122,.T.);
#3000=EDGE_CURVE('',#2467,#2468,#1526,.T.);
#3001=EDGE_CURVE('',#2468,#2469,#1527,.T.);
#3002=EDGE_CURVE('',#2469,#2470,#1528,.T.);
#3003=EDGE_CURVE('',#2470,#2471,#1529,.T.);
#3004=EDGE_CURVE('',#2471,#2472,#1530,.T.);
#3005=EDGE_CURVE('',#2472,#2467,#1531,.T.);
#3006=EDGE_CURVE('',#2473,#2473,#2123,.T.);
#3007=EDGE_CURVE('',#2467,#2461,#1532,.T.);
#3008=EDGE_CURVE('',#2462,#2472,#1533,.T.);
#3009=EDGE_CURVE('',#2463,#2471,#1534,.T.);
#3010=EDGE_CURVE('',#2464,#2470,#1535,.T.);
#3011=EDGE_CURVE('',#2465,#2469,#1536,.T.);
#3012=EDGE_CURVE('',#2460,#2468,#1537,.T.);
#3013=EDGE_CURVE('',#2473,#2474,#1538,.T.);
#3014=EDGE_CURVE('',#2474,#2474,#2124,.T.);
#3015=EDGE_CURVE('',#2475,#2475,#2125,.T.);
#3016=EDGE_CURVE('',#2476,#2476,#2126,.T.);
#3017=EDGE_CURVE('',#2474,#2475,#1539,.T.);
#3018=EDGE_CURVE('',#2477,#2477,#2127,.T.);
#3019=EDGE_CURVE('',#2477,#2466,#1540,.T.);
#3020=EDGE_CURVE('',#2478,#2478,#2128,.T.);
#3021=EDGE_CURVE('',#2478,#2477,#1541,.T.);
#3022=EDGE_CURVE('',#2479,#2479,#2129,.T.);
#3023=EDGE_CURVE('',#2479,#2476,#1542,.T.);
#3024=EDGE_CURVE('',#2480,#2480,#2130,.T.);
#3025=EDGE_CURVE('',#2481,#2481,#2131,.T.);
#3026=EDGE_CURVE('',#2481,#2480,#1543,.T.);
#3027=EDGE_CURVE('',#2482,#2482,#2132,.T.);
#3028=EDGE_CURVE('',#2482,#2481,#1544,.T.);
#3029=EDGE_CURVE('',#2483,#2483,#2133,.T.);
#3030=EDGE_CURVE('',#2483,#2482,#1545,.T.);
#3031=EDGE_CURVE('',#2484,#2484,#2134,.T.);
#3032=EDGE_CURVE('',#2485,#2485,#2135,.F.);
#3033=EDGE_CURVE('',#2485,#2484,#1546,.T.);
#3034=EDGE_CURVE('',#2486,#2486,#2136,.F.);
#3035=EDGE_CURVE('',#2486,#2485,#1547,.T.);
#3036=EDGE_CURVE('',#2487,#2487,#2137,.T.);
#3037=EDGE_CURVE('',#2487,#2486,#1548,.T.);
#3038=EDGE_CURVE('',#2488,#2489,#1549,.T.);
#3039=EDGE_CURVE('',#2489,#2490,#1550,.T.);
#3040=EDGE_CURVE('',#2490,#2491,#1551,.T.);
#3041=EDGE_CURVE('',#2488,#2491,#1552,.T.);
#3042=EDGE_CURVE('',#2489,#2492,#1553,.T.);
#3043=EDGE_CURVE('',#2492,#2493,#1554,.T.);
#3044=EDGE_CURVE('',#2493,#2490,#1555,.T.);
#3045=EDGE_CURVE('',#2492,#2494,#1556,.T.);
#3046=EDGE_CURVE('',#2494,#2495,#1557,.T.);
#3047=EDGE_CURVE('',#2495,#2493,#1558,.T.);
#3048=EDGE_CURVE('',#2494,#2496,#1559,.T.);
#3049=EDGE_CURVE('',#2496,#2497,#1560,.T.);
#3050=EDGE_CURVE('',#2497,#2495,#1561,.T.);
#3051=EDGE_CURVE('',#2496,#2498,#1562,.T.);
#3052=EDGE_CURVE('',#2498,#2499,#1563,.T.);
#3053=EDGE_CURVE('',#2499,#2497,#1564,.T.);
#3054=EDGE_CURVE('',#2498,#2488,#1565,.T.);
#3055=EDGE_CURVE('',#2491,#2499,#1566,.T.);
#3056=EDGE_CURVE('',#2500,#2501,#1567,.T.);
#3057=EDGE_CURVE('',#2501,#2502,#1568,.T.);
#3058=EDGE_CURVE('',#2502,#2503,#1569,.T.);
#3059=EDGE_CURVE('',#2500,#2503,#1570,.T.);
#3060=EDGE_CURVE('',#2501,#2504,#1571,.T.);
#3061=EDGE_CURVE('',#2504,#2505,#1572,.T.);
#3062=EDGE_CURVE('',#2505,#2502,#1573,.T.);
#3063=EDGE_CURVE('',#2504,#2506,#1574,.T.);
#3064=EDGE_CURVE('',#2506,#2507,#1575,.T.);
#3065=EDGE_CURVE('',#2507,#2505,#1576,.T.);
#3066=EDGE_CURVE('',#2506,#2508,#1577,.T.);
#3067=EDGE_CURVE('',#2508,#2509,#1578,.T.);
#3068=EDGE_CURVE('',#2509,#2507,#1579,.T.);
#3069=EDGE_CURVE('',#2508,#2510,#1580,.T.);
#3070=EDGE_CURVE('',#2510,#2511,#1581,.T.);
#3071=EDGE_CURVE('',#2511,#2509,#1582,.T.);
#3072=EDGE_CURVE('',#2510,#2500,#1583,.T.);
#3073=EDGE_CURVE('',#2503,#2511,#1584,.T.);
#3074=EDGE_CURVE('',#2512,#2512,#2138,.T.);
#3075=EDGE_CURVE('',#2513,#2513,#2139,.T.);
#3076=EDGE_CURVE('',#2514,#2514,#2140,.T.);
#3077=EDGE_CURVE('',#2514,#2513,#1585,.T.);
#3078=EDGE_CURVE('',#2515,#2515,#2141,.T.);
#3079=EDGE_CURVE('',#2515,#2514,#1586,.T.);
#3080=EDGE_CURVE('',#2516,#2516,#2142,.T.);
#3081=EDGE_CURVE('',#2516,#2515,#1587,.T.);
#3082=EDGE_CURVE('',#2517,#2517,#2143,.T.);
#3083=EDGE_CURVE('',#2518,#2518,#2144,.F.);
#3084=EDGE_CURVE('',#2518,#2517,#1588,.T.);
#3085=EDGE_CURVE('',#2512,#2518,#1589,.T.);
#3086=ORIENTED_EDGE('',*,*,#2519,.F.);
#3087=ORIENTED_EDGE('',*,*,#2520,.T.);
#3088=ORIENTED_EDGE('',*,*,#2521,.F.);
#3089=ORIENTED_EDGE('',*,*,#2520,.F.);
#3090=ORIENTED_EDGE('',*,*,#2519,.T.);
#3091=ORIENTED_EDGE('',*,*,#2522,.F.);
#3092=ORIENTED_EDGE('',*,*,#2523,.T.);
#3093=ORIENTED_EDGE('',*,*,#2524,.F.);
#3094=ORIENTED_EDGE('',*,*,#2523,.F.);
#3095=ORIENTED_EDGE('',*,*,#2522,.T.);
#3096=ORIENTED_EDGE('',*,*,#2525,.F.);
#3097=ORIENTED_EDGE('',*,*,#2526,.T.);
#3098=ORIENTED_EDGE('',*,*,#2527,.F.);
#3099=ORIENTED_EDGE('',*,*,#2526,.F.);
#3100=ORIENTED_EDGE('',*,*,#2525,.T.);
#3101=ORIENTED_EDGE('',*,*,#2528,.F.);
#3102=ORIENTED_EDGE('',*,*,#2529,.T.);
#3103=ORIENTED_EDGE('',*,*,#2530,.F.);
#3104=ORIENTED_EDGE('',*,*,#2529,.F.);
#3105=ORIENTED_EDGE('',*,*,#2528,.T.);
#3106=ORIENTED_EDGE('',*,*,#2531,.F.);
#3107=ORIENTED_EDGE('',*,*,#2532,.T.);
#3108=ORIENTED_EDGE('',*,*,#2533,.F.);
#3109=ORIENTED_EDGE('',*,*,#2532,.F.);
#3110=ORIENTED_EDGE('',*,*,#2534,.F.);
#3111=ORIENTED_EDGE('',*,*,#2535,.T.);
#3112=ORIENTED_EDGE('',*,*,#2536,.F.);
#3113=ORIENTED_EDGE('',*,*,#2535,.F.);
#3114=ORIENTED_EDGE('',*,*,#2537,.F.);
#3115=ORIENTED_EDGE('',*,*,#2538,.T.);
#3116=ORIENTED_EDGE('',*,*,#2539,.F.);
#3117=ORIENTED_EDGE('',*,*,#2538,.F.);
#3118=ORIENTED_EDGE('',*,*,#2540,.F.);
#3119=ORIENTED_EDGE('',*,*,#2541,.T.);
#3120=ORIENTED_EDGE('',*,*,#2542,.F.);
#3121=ORIENTED_EDGE('',*,*,#2541,.F.);
#3122=ORIENTED_EDGE('',*,*,#2543,.T.);
#3123=ORIENTED_EDGE('',*,*,#2544,.T.);
#3124=ORIENTED_EDGE('',*,*,#2545,.F.);
#3125=ORIENTED_EDGE('',*,*,#2546,.F.);
#3126=ORIENTED_EDGE('',*,*,#2547,.T.);
#3127=ORIENTED_EDGE('',*,*,#2546,.T.);
#3128=ORIENTED_EDGE('',*,*,#2548,.F.);
#3129=ORIENTED_EDGE('',*,*,#2549,.F.);
#3130=ORIENTED_EDGE('',*,*,#2550,.T.);
#3131=ORIENTED_EDGE('',*,*,#2549,.T.);
#3132=ORIENTED_EDGE('',*,*,#2551,.F.);
#3133=ORIENTED_EDGE('',*,*,#2552,.F.);
#3134=ORIENTED_EDGE('',*,*,#2553,.T.);
#3135=ORIENTED_EDGE('',*,*,#2552,.T.);
#3136=ORIENTED_EDGE('',*,*,#2554,.F.);
#3137=ORIENTED_EDGE('',*,*,#2544,.F.);
#3138=ORIENTED_EDGE('',*,*,#2554,.T.);
#3139=ORIENTED_EDGE('',*,*,#2551,.T.);
#3140=ORIENTED_EDGE('',*,*,#2548,.T.);
#3141=ORIENTED_EDGE('',*,*,#2545,.T.);
#3142=ORIENTED_EDGE('',*,*,#2542,.T.);
#3143=ORIENTED_EDGE('',*,*,#2539,.T.);
#3144=ORIENTED_EDGE('',*,*,#2536,.T.);
#3145=ORIENTED_EDGE('',*,*,#2533,.T.);
#3146=ORIENTED_EDGE('',*,*,#2530,.T.);
#3147=ORIENTED_EDGE('',*,*,#2527,.T.);
#3148=ORIENTED_EDGE('',*,*,#2524,.T.);
#3149=ORIENTED_EDGE('',*,*,#2521,.T.);
#3150=ORIENTED_EDGE('',*,*,#2553,.F.);
#3151=ORIENTED_EDGE('',*,*,#2543,.F.);
#3152=ORIENTED_EDGE('',*,*,#2547,.F.);
#3153=ORIENTED_EDGE('',*,*,#2550,.F.);
#3154=ORIENTED_EDGE('',*,*,#2531,.T.);
#3155=ORIENTED_EDGE('',*,*,#2534,.T.);
#3156=ORIENTED_EDGE('',*,*,#2537,.T.);
#3157=ORIENTED_EDGE('',*,*,#2540,.T.);
#3158=ORIENTED_EDGE('',*,*,#2555,.T.);
#3159=ORIENTED_EDGE('',*,*,#2556,.T.);
#3160=ORIENTED_EDGE('',*,*,#2557,.F.);
#3161=ORIENTED_EDGE('',*,*,#2558,.F.);
#3162=ORIENTED_EDGE('',*,*,#2559,.T.);
#3163=ORIENTED_EDGE('',*,*,#2558,.T.);
#3164=ORIENTED_EDGE('',*,*,#2560,.F.);
#3165=ORIENTED_EDGE('',*,*,#2561,.F.);
#3166=ORIENTED_EDGE('',*,*,#2562,.T.);
#3167=ORIENTED_EDGE('',*,*,#2561,.T.);
#3168=ORIENTED_EDGE('',*,*,#2563,.F.);
#3169=ORIENTED_EDGE('',*,*,#2564,.F.);
#3170=ORIENTED_EDGE('',*,*,#2565,.T.);
#3171=ORIENTED_EDGE('',*,*,#2564,.T.);
#3172=ORIENTED_EDGE('',*,*,#2566,.F.);
#3173=ORIENTED_EDGE('',*,*,#2556,.F.);
#3174=ORIENTED_EDGE('',*,*,#2566,.T.);
#3175=ORIENTED_EDGE('',*,*,#2563,.T.);
#3176=ORIENTED_EDGE('',*,*,#2560,.T.);
#3177=ORIENTED_EDGE('',*,*,#2557,.T.);
#3178=ORIENTED_EDGE('',*,*,#2565,.F.);
#3179=ORIENTED_EDGE('',*,*,#2555,.F.);
#3180=ORIENTED_EDGE('',*,*,#2559,.F.);
#3181=ORIENTED_EDGE('',*,*,#2562,.F.);
#3182=ORIENTED_EDGE('',*,*,#2567,.T.);
#3183=ORIENTED_EDGE('',*,*,#2568,.T.);
#3184=ORIENTED_EDGE('',*,*,#2569,.F.);
#3185=ORIENTED_EDGE('',*,*,#2570,.F.);
#3186=ORIENTED_EDGE('',*,*,#2571,.T.);
#3187=ORIENTED_EDGE('',*,*,#2570,.T.);
#3188=ORIENTED_EDGE('',*,*,#2572,.F.);
#3189=ORIENTED_EDGE('',*,*,#2573,.F.);
#3190=ORIENTED_EDGE('',*,*,#2574,.T.);
#3191=ORIENTED_EDGE('',*,*,#2573,.T.);
#3192=ORIENTED_EDGE('',*,*,#2575,.F.);
#3193=ORIENTED_EDGE('',*,*,#2576,.F.);
#3194=ORIENTED_EDGE('',*,*,#2577,.T.);
#3195=ORIENTED_EDGE('',*,*,#2576,.T.);
#3196=ORIENTED_EDGE('',*,*,#2578,.F.);
#3197=ORIENTED_EDGE('',*,*,#2568,.F.);
#3198=ORIENTED_EDGE('',*,*,#2578,.T.);
#3199=ORIENTED_EDGE('',*,*,#2575,.T.);
#3200=ORIENTED_EDGE('',*,*,#2572,.T.);
#3201=ORIENTED_EDGE('',*,*,#2569,.T.);
#3202=ORIENTED_EDGE('',*,*,#2577,.F.);
#3203=ORIENTED_EDGE('',*,*,#2567,.F.);
#3204=ORIENTED_EDGE('',*,*,#2571,.F.);
#3205=ORIENTED_EDGE('',*,*,#2574,.F.);
#3206=ORIENTED_EDGE('',*,*,#2579,.F.);
#3207=ORIENTED_EDGE('',*,*,#2580,.T.);
#3208=ORIENTED_EDGE('',*,*,#2581,.F.);
#3209=ORIENTED_EDGE('',*,*,#2582,.F.);
#3210=ORIENTED_EDGE('',*,*,#2583,.F.);
#3211=ORIENTED_EDGE('',*,*,#2580,.F.);
#3212=ORIENTED_EDGE('',*,*,#2584,.F.);
#3213=ORIENTED_EDGE('',*,*,#2585,.T.);
#3214=ORIENTED_EDGE('',*,*,#2586,.F.);
#3215=ORIENTED_EDGE('',*,*,#2587,.F.);
#3216=ORIENTED_EDGE('',*,*,#2588,.F.);
#3217=ORIENTED_EDGE('',*,*,#2585,.F.);
#3218=ORIENTED_EDGE('',*,*,#2589,.F.);
#3219=ORIENTED_EDGE('',*,*,#2590,.T.);
#3220=ORIENTED_EDGE('',*,*,#2591,.F.);
#3221=ORIENTED_EDGE('',*,*,#2581,.T.);
#3222=ORIENTED_EDGE('',*,*,#2579,.T.);
#3223=ORIENTED_EDGE('',*,*,#2583,.T.);
#3224=ORIENTED_EDGE('',*,*,#2592,.F.);
#3225=ORIENTED_EDGE('',*,*,#2590,.F.);
#3226=ORIENTED_EDGE('',*,*,#2593,.F.);
#3227=ORIENTED_EDGE('',*,*,#2594,.T.);
#3228=ORIENTED_EDGE('',*,*,#2595,.F.);
#3229=ORIENTED_EDGE('',*,*,#2586,.T.);
#3230=ORIENTED_EDGE('',*,*,#2584,.T.);
#3231=ORIENTED_EDGE('',*,*,#2588,.T.);
#3232=ORIENTED_EDGE('',*,*,#2596,.F.);
#3233=ORIENTED_EDGE('',*,*,#2594,.F.);
#3234=ORIENTED_EDGE('',*,*,#2597,.F.);
#3235=ORIENTED_EDGE('',*,*,#2598,.T.);
#3236=ORIENTED_EDGE('',*,*,#2599,.F.);
#3237=ORIENTED_EDGE('',*,*,#2598,.F.);
#3238=ORIENTED_EDGE('',*,*,#2600,.F.);
#3239=ORIENTED_EDGE('',*,*,#2601,.T.);
#3240=ORIENTED_EDGE('',*,*,#2602,.F.);
#3241=ORIENTED_EDGE('',*,*,#2601,.F.);
#3242=ORIENTED_EDGE('',*,*,#2603,.T.);
#3243=ORIENTED_EDGE('',*,*,#2604,.T.);
#3244=ORIENTED_EDGE('',*,*,#2605,.F.);
#3245=ORIENTED_EDGE('',*,*,#2606,.F.);
#3246=ORIENTED_EDGE('',*,*,#2607,.T.);
#3247=ORIENTED_EDGE('',*,*,#2606,.T.);
#3248=ORIENTED_EDGE('',*,*,#2608,.F.);
#3249=ORIENTED_EDGE('',*,*,#2609,.F.);
#3250=ORIENTED_EDGE('',*,*,#2610,.T.);
#3251=ORIENTED_EDGE('',*,*,#2609,.T.);
#3252=ORIENTED_EDGE('',*,*,#2611,.F.);
#3253=ORIENTED_EDGE('',*,*,#2612,.F.);
#3254=ORIENTED_EDGE('',*,*,#2613,.T.);
#3255=ORIENTED_EDGE('',*,*,#2612,.T.);
#3256=ORIENTED_EDGE('',*,*,#2614,.F.);
#3257=ORIENTED_EDGE('',*,*,#2604,.F.);
#3258=ORIENTED_EDGE('',*,*,#2614,.T.);
#3259=ORIENTED_EDGE('',*,*,#2611,.T.);
#3260=ORIENTED_EDGE('',*,*,#2608,.T.);
#3261=ORIENTED_EDGE('',*,*,#2605,.T.);
#3262=ORIENTED_EDGE('',*,*,#2582,.T.);
#3263=ORIENTED_EDGE('',*,*,#2591,.T.);
#3264=ORIENTED_EDGE('',*,*,#2592,.T.);
#3265=ORIENTED_EDGE('',*,*,#2587,.T.);
#3266=ORIENTED_EDGE('',*,*,#2595,.T.);
#3267=ORIENTED_EDGE('',*,*,#2596,.T.);
#3268=ORIENTED_EDGE('',*,*,#2599,.T.);
#3269=ORIENTED_EDGE('',*,*,#2602,.T.);
#3270=ORIENTED_EDGE('',*,*,#2613,.F.);
#3271=ORIENTED_EDGE('',*,*,#2603,.F.);
#3272=ORIENTED_EDGE('',*,*,#2607,.F.);
#3273=ORIENTED_EDGE('',*,*,#2610,.F.);
#3274=ORIENTED_EDGE('',*,*,#2589,.T.);
#3275=ORIENTED_EDGE('',*,*,#2597,.T.);
#3276=ORIENTED_EDGE('',*,*,#2600,.T.);
#3277=ORIENTED_EDGE('',*,*,#2593,.T.);
#3278=ORIENTED_EDGE('',*,*,#2615,.F.);
#3279=ORIENTED_EDGE('',*,*,#2616,.T.);
#3280=ORIENTED_EDGE('',*,*,#2617,.F.);
#3281=ORIENTED_EDGE('',*,*,#2618,.F.);
#3282=ORIENTED_EDGE('',*,*,#2619,.F.);
#3283=ORIENTED_EDGE('',*,*,#2616,.F.);
#3284=ORIENTED_EDGE('',*,*,#2620,.F.);
#3285=ORIENTED_EDGE('',*,*,#2621,.T.);
#3286=ORIENTED_EDGE('',*,*,#2622,.F.);
#3287=ORIENTED_EDGE('',*,*,#2623,.F.);
#3288=ORIENTED_EDGE('',*,*,#2624,.F.);
#3289=ORIENTED_EDGE('',*,*,#2621,.F.);
#3290=ORIENTED_EDGE('',*,*,#2625,.F.);
#3291=ORIENTED_EDGE('',*,*,#2626,.T.);
#3292=ORIENTED_EDGE('',*,*,#2627,.F.);
#3293=ORIENTED_EDGE('',*,*,#2617,.T.);
#3294=ORIENTED_EDGE('',*,*,#2615,.T.);
#3295=ORIENTED_EDGE('',*,*,#2619,.T.);
#3296=ORIENTED_EDGE('',*,*,#2628,.F.);
#3297=ORIENTED_EDGE('',*,*,#2626,.F.);
#3298=ORIENTED_EDGE('',*,*,#2629,.F.);
#3299=ORIENTED_EDGE('',*,*,#2630,.T.);
#3300=ORIENTED_EDGE('',*,*,#2631,.F.);
#3301=ORIENTED_EDGE('',*,*,#2622,.T.);
#3302=ORIENTED_EDGE('',*,*,#2620,.T.);
#3303=ORIENTED_EDGE('',*,*,#2624,.T.);
#3304=ORIENTED_EDGE('',*,*,#2632,.F.);
#3305=ORIENTED_EDGE('',*,*,#2630,.F.);
#3306=ORIENTED_EDGE('',*,*,#2633,.F.);
#3307=ORIENTED_EDGE('',*,*,#2634,.T.);
#3308=ORIENTED_EDGE('',*,*,#2635,.F.);
#3309=ORIENTED_EDGE('',*,*,#2634,.F.);
#3310=ORIENTED_EDGE('',*,*,#2636,.F.);
#3311=ORIENTED_EDGE('',*,*,#2637,.T.);
#3312=ORIENTED_EDGE('',*,*,#2638,.F.);
#3313=ORIENTED_EDGE('',*,*,#2637,.F.);
#3314=ORIENTED_EDGE('',*,*,#2639,.T.);
#3315=ORIENTED_EDGE('',*,*,#2640,.T.);
#3316=ORIENTED_EDGE('',*,*,#2641,.F.);
#3317=ORIENTED_EDGE('',*,*,#2642,.F.);
#3318=ORIENTED_EDGE('',*,*,#2643,.T.);
#3319=ORIENTED_EDGE('',*,*,#2642,.T.);
#3320=ORIENTED_EDGE('',*,*,#2644,.F.);
#3321=ORIENTED_EDGE('',*,*,#2645,.F.);
#3322=ORIENTED_EDGE('',*,*,#2646,.T.);
#3323=ORIENTED_EDGE('',*,*,#2645,.T.);
#3324=ORIENTED_EDGE('',*,*,#2647,.F.);
#3325=ORIENTED_EDGE('',*,*,#2648,.F.);
#3326=ORIENTED_EDGE('',*,*,#2649,.T.);
#3327=ORIENTED_EDGE('',*,*,#2648,.T.);
#3328=ORIENTED_EDGE('',*,*,#2650,.F.);
#3329=ORIENTED_EDGE('',*,*,#2640,.F.);
#3330=ORIENTED_EDGE('',*,*,#2650,.T.);
#3331=ORIENTED_EDGE('',*,*,#2647,.T.);
#3332=ORIENTED_EDGE('',*,*,#2644,.T.);
#3333=ORIENTED_EDGE('',*,*,#2641,.T.);
#3334=ORIENTED_EDGE('',*,*,#2618,.T.);
#3335=ORIENTED_EDGE('',*,*,#2627,.T.);
#3336=ORIENTED_EDGE('',*,*,#2628,.T.);
#3337=ORIENTED_EDGE('',*,*,#2623,.T.);
#3338=ORIENTED_EDGE('',*,*,#2631,.T.);
#3339=ORIENTED_EDGE('',*,*,#2632,.T.);
#3340=ORIENTED_EDGE('',*,*,#2635,.T.);
#3341=ORIENTED_EDGE('',*,*,#2638,.T.);
#3342=ORIENTED_EDGE('',*,*,#2649,.F.);
#3343=ORIENTED_EDGE('',*,*,#2639,.F.);
#3344=ORIENTED_EDGE('',*,*,#2643,.F.);
#3345=ORIENTED_EDGE('',*,*,#2646,.F.);
#3346=ORIENTED_EDGE('',*,*,#2625,.T.);
#3347=ORIENTED_EDGE('',*,*,#2633,.T.);
#3348=ORIENTED_EDGE('',*,*,#2636,.T.);
#3349=ORIENTED_EDGE('',*,*,#2629,.T.);
#3350=ORIENTED_EDGE('',*,*,#2651,.F.);
#3351=ORIENTED_EDGE('',*,*,#2652,.T.);
#3352=ORIENTED_EDGE('',*,*,#2653,.F.);
#3353=ORIENTED_EDGE('',*,*,#2652,.F.);
#3354=ORIENTED_EDGE('',*,*,#2654,.F.);
#3355=ORIENTED_EDGE('',*,*,#2655,.T.);
#3356=ORIENTED_EDGE('',*,*,#2656,.F.);
#3357=ORIENTED_EDGE('',*,*,#2655,.F.);
#3358=ORIENTED_EDGE('',*,*,#2657,.F.);
#3359=ORIENTED_EDGE('',*,*,#2658,.T.);
#3360=ORIENTED_EDGE('',*,*,#2659,.F.);
#3361=ORIENTED_EDGE('',*,*,#2658,.F.);
#3362=ORIENTED_EDGE('',*,*,#2660,.F.);
#3363=ORIENTED_EDGE('',*,*,#2661,.T.);
#3364=ORIENTED_EDGE('',*,*,#2662,.F.);
#3365=ORIENTED_EDGE('',*,*,#2661,.F.);
#3366=ORIENTED_EDGE('',*,*,#2663,.F.);
#3367=ORIENTED_EDGE('',*,*,#2664,.T.);
#3368=ORIENTED_EDGE('',*,*,#2665,.F.);
#3369=ORIENTED_EDGE('',*,*,#2664,.F.);
#3370=ORIENTED_EDGE('',*,*,#2666,.F.);
#3371=ORIENTED_EDGE('',*,*,#2667,.T.);
#3372=ORIENTED_EDGE('',*,*,#2668,.F.);
#3373=ORIENTED_EDGE('',*,*,#2667,.F.);
#3374=ORIENTED_EDGE('',*,*,#2669,.F.);
#3375=ORIENTED_EDGE('',*,*,#2670,.T.);
#3376=ORIENTED_EDGE('',*,*,#2671,.F.);
#3377=ORIENTED_EDGE('',*,*,#2670,.F.);
#3378=ORIENTED_EDGE('',*,*,#2672,.F.);
#3379=ORIENTED_EDGE('',*,*,#2673,.T.);
#3380=ORIENTED_EDGE('',*,*,#2674,.F.);
#3381=ORIENTED_EDGE('',*,*,#2673,.F.);
#3382=ORIENTED_EDGE('',*,*,#2675,.F.);
#3383=ORIENTED_EDGE('',*,*,#2676,.T.);
#3384=ORIENTED_EDGE('',*,*,#2677,.F.);
#3385=ORIENTED_EDGE('',*,*,#2676,.F.);
#3386=ORIENTED_EDGE('',*,*,#2678,.F.);
#3387=ORIENTED_EDGE('',*,*,#2679,.T.);
#3388=ORIENTED_EDGE('',*,*,#2680,.F.);
#3389=ORIENTED_EDGE('',*,*,#2679,.F.);
#3390=ORIENTED_EDGE('',*,*,#2681,.F.);
#3391=ORIENTED_EDGE('',*,*,#2682,.T.);
#3392=ORIENTED_EDGE('',*,*,#2683,.F.);
#3393=ORIENTED_EDGE('',*,*,#2682,.F.);
#3394=ORIENTED_EDGE('',*,*,#2684,.F.);
#3395=ORIENTED_EDGE('',*,*,#2685,.T.);
#3396=ORIENTED_EDGE('',*,*,#2686,.F.);
#3397=ORIENTED_EDGE('',*,*,#2685,.F.);
#3398=ORIENTED_EDGE('',*,*,#2687,.T.);
#3399=ORIENTED_EDGE('',*,*,#2688,.T.);
#3400=ORIENTED_EDGE('',*,*,#2689,.F.);
#3401=ORIENTED_EDGE('',*,*,#2690,.F.);
#3402=ORIENTED_EDGE('',*,*,#2691,.T.);
#3403=ORIENTED_EDGE('',*,*,#2690,.T.);
#3404=ORIENTED_EDGE('',*,*,#2692,.F.);
#3405=ORIENTED_EDGE('',*,*,#2693,.F.);
#3406=ORIENTED_EDGE('',*,*,#2694,.T.);
#3407=ORIENTED_EDGE('',*,*,#2693,.T.);
#3408=ORIENTED_EDGE('',*,*,#2695,.F.);
#3409=ORIENTED_EDGE('',*,*,#2696,.F.);
#3410=ORIENTED_EDGE('',*,*,#2697,.T.);
#3411=ORIENTED_EDGE('',*,*,#2696,.T.);
#3412=ORIENTED_EDGE('',*,*,#2698,.F.);
#3413=ORIENTED_EDGE('',*,*,#2688,.F.);
#3414=ORIENTED_EDGE('',*,*,#2698,.T.);
#3415=ORIENTED_EDGE('',*,*,#2695,.T.);
#3416=ORIENTED_EDGE('',*,*,#2692,.T.);
#3417=ORIENTED_EDGE('',*,*,#2689,.T.);
#3418=ORIENTED_EDGE('',*,*,#2656,.T.);
#3419=ORIENTED_EDGE('',*,*,#2686,.T.);
#3420=ORIENTED_EDGE('',*,*,#2683,.T.);
#3421=ORIENTED_EDGE('',*,*,#2680,.T.);
#3422=ORIENTED_EDGE('',*,*,#2677,.T.);
#3423=ORIENTED_EDGE('',*,*,#2674,.T.);
#3424=ORIENTED_EDGE('',*,*,#2671,.T.);
#3425=ORIENTED_EDGE('',*,*,#2668,.T.);
#3426=ORIENTED_EDGE('',*,*,#2665,.T.);
#3427=ORIENTED_EDGE('',*,*,#2662,.T.);
#3428=ORIENTED_EDGE('',*,*,#2659,.T.);
#3429=ORIENTED_EDGE('',*,*,#2653,.T.);
#3430=ORIENTED_EDGE('',*,*,#2697,.F.);
#3431=ORIENTED_EDGE('',*,*,#2687,.F.);
#3432=ORIENTED_EDGE('',*,*,#2691,.F.);
#3433=ORIENTED_EDGE('',*,*,#2694,.F.);
#3434=ORIENTED_EDGE('',*,*,#2654,.T.);
#3435=ORIENTED_EDGE('',*,*,#2684,.T.);
#3436=ORIENTED_EDGE('',*,*,#2681,.T.);
#3437=ORIENTED_EDGE('',*,*,#2678,.T.);
#3438=ORIENTED_EDGE('',*,*,#2675,.T.);
#3439=ORIENTED_EDGE('',*,*,#2672,.T.);
#3440=ORIENTED_EDGE('',*,*,#2669,.T.);
#3441=ORIENTED_EDGE('',*,*,#2666,.T.);
#3442=ORIENTED_EDGE('',*,*,#2663,.T.);
#3443=ORIENTED_EDGE('',*,*,#2660,.T.);
#3444=ORIENTED_EDGE('',*,*,#2657,.T.);
#3445=ORIENTED_EDGE('',*,*,#2651,.T.);
#3446=ORIENTED_EDGE('',*,*,#2699,.F.);
#3447=ORIENTED_EDGE('',*,*,#2700,.T.);
#3448=ORIENTED_EDGE('',*,*,#2701,.F.);
#3449=ORIENTED_EDGE('',*,*,#2700,.F.);
#3450=ORIENTED_EDGE('',*,*,#2702,.F.);
#3451=ORIENTED_EDGE('',*,*,#2703,.T.);
#3452=ORIENTED_EDGE('',*,*,#2704,.F.);
#3453=ORIENTED_EDGE('',*,*,#2703,.F.);
#3454=ORIENTED_EDGE('',*,*,#2705,.F.);
#3455=ORIENTED_EDGE('',*,*,#2706,.T.);
#3456=ORIENTED_EDGE('',*,*,#2707,.F.);
#3457=ORIENTED_EDGE('',*,*,#2706,.F.);
#3458=ORIENTED_EDGE('',*,*,#2708,.F.);
#3459=ORIENTED_EDGE('',*,*,#2709,.T.);
#3460=ORIENTED_EDGE('',*,*,#2710,.F.);
#3461=ORIENTED_EDGE('',*,*,#2709,.F.);
#3462=ORIENTED_EDGE('',*,*,#2711,.F.);
#3463=ORIENTED_EDGE('',*,*,#2712,.T.);
#3464=ORIENTED_EDGE('',*,*,#2713,.F.);
#3465=ORIENTED_EDGE('',*,*,#2712,.F.);
#3466=ORIENTED_EDGE('',*,*,#2714,.F.);
#3467=ORIENTED_EDGE('',*,*,#2715,.T.);
#3468=ORIENTED_EDGE('',*,*,#2716,.F.);
#3469=ORIENTED_EDGE('',*,*,#2715,.F.);
#3470=ORIENTED_EDGE('',*,*,#2717,.F.);
#3471=ORIENTED_EDGE('',*,*,#2718,.T.);
#3472=ORIENTED_EDGE('',*,*,#2719,.F.);
#3473=ORIENTED_EDGE('',*,*,#2718,.F.);
#3474=ORIENTED_EDGE('',*,*,#2720,.F.);
#3475=ORIENTED_EDGE('',*,*,#2721,.T.);
#3476=ORIENTED_EDGE('',*,*,#2722,.F.);
#3477=ORIENTED_EDGE('',*,*,#2721,.F.);
#3478=ORIENTED_EDGE('',*,*,#2723,.F.);
#3479=ORIENTED_EDGE('',*,*,#2724,.F.);
#3480=ORIENTED_EDGE('',*,*,#2725,.F.);
#3481=ORIENTED_EDGE('',*,*,#2726,.T.);
#3482=ORIENTED_EDGE('',*,*,#2727,.F.);
#3483=ORIENTED_EDGE('',*,*,#2726,.F.);
#3484=ORIENTED_EDGE('',*,*,#2728,.F.);
#3485=ORIENTED_EDGE('',*,*,#2729,.T.);
#3486=ORIENTED_EDGE('',*,*,#2730,.F.);
#3487=ORIENTED_EDGE('',*,*,#2729,.F.);
#3488=ORIENTED_EDGE('',*,*,#2731,.F.);
#3489=ORIENTED_EDGE('',*,*,#2732,.T.);
#3490=ORIENTED_EDGE('',*,*,#2733,.F.);
#3491=ORIENTED_EDGE('',*,*,#2732,.F.);
#3492=ORIENTED_EDGE('',*,*,#2734,.F.);
#3493=ORIENTED_EDGE('',*,*,#2724,.T.);
#3494=ORIENTED_EDGE('',*,*,#2735,.T.);
#3495=ORIENTED_EDGE('',*,*,#2736,.T.);
#3496=ORIENTED_EDGE('',*,*,#2737,.F.);
#3497=ORIENTED_EDGE('',*,*,#2738,.F.);
#3498=ORIENTED_EDGE('',*,*,#2739,.T.);
#3499=ORIENTED_EDGE('',*,*,#2738,.T.);
#3500=ORIENTED_EDGE('',*,*,#2740,.F.);
#3501=ORIENTED_EDGE('',*,*,#2741,.F.);
#3502=ORIENTED_EDGE('',*,*,#2742,.T.);
#3503=ORIENTED_EDGE('',*,*,#2741,.T.);
#3504=ORIENTED_EDGE('',*,*,#2743,.F.);
#3505=ORIENTED_EDGE('',*,*,#2744,.F.);
#3506=ORIENTED_EDGE('',*,*,#2745,.T.);
#3507=ORIENTED_EDGE('',*,*,#2744,.T.);
#3508=ORIENTED_EDGE('',*,*,#2746,.F.);
#3509=ORIENTED_EDGE('',*,*,#2736,.F.);
#3510=ORIENTED_EDGE('',*,*,#2746,.T.);
#3511=ORIENTED_EDGE('',*,*,#2743,.T.);
#3512=ORIENTED_EDGE('',*,*,#2740,.T.);
#3513=ORIENTED_EDGE('',*,*,#2737,.T.);
#3514=ORIENTED_EDGE('',*,*,#2704,.T.);
#3515=ORIENTED_EDGE('',*,*,#2730,.T.);
#3516=ORIENTED_EDGE('',*,*,#2733,.T.);
#3517=ORIENTED_EDGE('',*,*,#2723,.T.);
#3518=ORIENTED_EDGE('',*,*,#2727,.T.);
#3519=ORIENTED_EDGE('',*,*,#2722,.T.);
#3520=ORIENTED_EDGE('',*,*,#2719,.T.);
#3521=ORIENTED_EDGE('',*,*,#2716,.T.);
#3522=ORIENTED_EDGE('',*,*,#2713,.T.);
#3523=ORIENTED_EDGE('',*,*,#2710,.T.);
#3524=ORIENTED_EDGE('',*,*,#2707,.T.);
#3525=ORIENTED_EDGE('',*,*,#2701,.T.);
#3526=ORIENTED_EDGE('',*,*,#2745,.F.);
#3527=ORIENTED_EDGE('',*,*,#2735,.F.);
#3528=ORIENTED_EDGE('',*,*,#2739,.F.);
#3529=ORIENTED_EDGE('',*,*,#2742,.F.);
#3530=ORIENTED_EDGE('',*,*,#2702,.T.);
#3531=ORIENTED_EDGE('',*,*,#2731,.T.);
#3532=ORIENTED_EDGE('',*,*,#2728,.T.);
#3533=ORIENTED_EDGE('',*,*,#2725,.T.);
#3534=ORIENTED_EDGE('',*,*,#2734,.T.);
#3535=ORIENTED_EDGE('',*,*,#2720,.T.);
#3536=ORIENTED_EDGE('',*,*,#2717,.T.);
#3537=ORIENTED_EDGE('',*,*,#2714,.T.);
#3538=ORIENTED_EDGE('',*,*,#2711,.T.);
#3539=ORIENTED_EDGE('',*,*,#2708,.T.);
#3540=ORIENTED_EDGE('',*,*,#2705,.T.);
#3541=ORIENTED_EDGE('',*,*,#2699,.T.);
#3542=ORIENTED_EDGE('',*,*,#2747,.F.);
#3543=ORIENTED_EDGE('',*,*,#2748,.T.);
#3544=ORIENTED_EDGE('',*,*,#2749,.T.);
#3545=ORIENTED_EDGE('',*,*,#2748,.F.);
#3546=ORIENTED_EDGE('',*,*,#2749,.F.);
#3547=ORIENTED_EDGE('',*,*,#2750,.F.);
#3548=ORIENTED_EDGE('',*,*,#2751,.T.);
#3549=ORIENTED_EDGE('',*,*,#2752,.T.);
#3550=ORIENTED_EDGE('',*,*,#2751,.F.);
#3551=ORIENTED_EDGE('',*,*,#2752,.F.);
#3552=ORIENTED_EDGE('',*,*,#2753,.F.);
#3553=ORIENTED_EDGE('',*,*,#2754,.T.);
#3554=ORIENTED_EDGE('',*,*,#2755,.T.);
#3555=ORIENTED_EDGE('',*,*,#2754,.F.);
#3556=ORIENTED_EDGE('',*,*,#2755,.F.);
#3557=ORIENTED_EDGE('',*,*,#2756,.F.);
#3558=ORIENTED_EDGE('',*,*,#2757,.T.);
#3559=ORIENTED_EDGE('',*,*,#2758,.T.);
#3560=ORIENTED_EDGE('',*,*,#2757,.F.);
#3561=ORIENTED_EDGE('',*,*,#2758,.F.);
#3562=ORIENTED_EDGE('',*,*,#2759,.F.);
#3563=ORIENTED_EDGE('',*,*,#2760,.T.);
#3564=ORIENTED_EDGE('',*,*,#2761,.T.);
#3565=ORIENTED_EDGE('',*,*,#2760,.F.);
#3566=ORIENTED_EDGE('',*,*,#2761,.F.);
#3567=ORIENTED_EDGE('',*,*,#2762,.F.);
#3568=ORIENTED_EDGE('',*,*,#2763,.T.);
#3569=ORIENTED_EDGE('',*,*,#2764,.T.);
#3570=ORIENTED_EDGE('',*,*,#2763,.F.);
#3571=ORIENTED_EDGE('',*,*,#2764,.F.);
#3572=ORIENTED_EDGE('',*,*,#2765,.F.);
#3573=ORIENTED_EDGE('',*,*,#2766,.T.);
#3574=ORIENTED_EDGE('',*,*,#2767,.T.);
#3575=ORIENTED_EDGE('',*,*,#2766,.F.);
#3576=ORIENTED_EDGE('',*,*,#2767,.F.);
#3577=ORIENTED_EDGE('',*,*,#2768,.F.);
#3578=ORIENTED_EDGE('',*,*,#2769,.T.);
#3579=ORIENTED_EDGE('',*,*,#2770,.T.);
#3580=ORIENTED_EDGE('',*,*,#2769,.F.);
#3581=ORIENTED_EDGE('',*,*,#2770,.F.);
#3582=ORIENTED_EDGE('',*,*,#2771,.F.);
#3583=ORIENTED_EDGE('',*,*,#2772,.T.);
#3584=ORIENTED_EDGE('',*,*,#2773,.T.);
#3585=ORIENTED_EDGE('',*,*,#2772,.F.);
#3586=ORIENTED_EDGE('',*,*,#2773,.F.);
#3587=ORIENTED_EDGE('',*,*,#2774,.F.);
#3588=ORIENTED_EDGE('',*,*,#2775,.T.);
#3589=ORIENTED_EDGE('',*,*,#2776,.T.);
#3590=ORIENTED_EDGE('',*,*,#2775,.F.);
#3591=ORIENTED_EDGE('',*,*,#2776,.F.);
#3592=ORIENTED_EDGE('',*,*,#2777,.F.);
#3593=ORIENTED_EDGE('',*,*,#2778,.T.);
#3594=ORIENTED_EDGE('',*,*,#2779,.F.);
#3595=ORIENTED_EDGE('',*,*,#2778,.F.);
#3596=ORIENTED_EDGE('',*,*,#2777,.T.);
#3597=ORIENTED_EDGE('',*,*,#2780,.F.);
#3598=ORIENTED_EDGE('',*,*,#2781,.F.);
#3599=ORIENTED_EDGE('',*,*,#2782,.T.);
#3600=ORIENTED_EDGE('',*,*,#2783,.T.);
#3601=ORIENTED_EDGE('',*,*,#2782,.F.);
#3602=ORIENTED_EDGE('',*,*,#2783,.F.);
#3603=ORIENTED_EDGE('',*,*,#2784,.F.);
#3604=ORIENTED_EDGE('',*,*,#2785,.F.);
#3605=ORIENTED_EDGE('',*,*,#2786,.F.);
#3606=ORIENTED_EDGE('',*,*,#2787,.T.);
#3607=ORIENTED_EDGE('',*,*,#2788,.F.);
#3608=ORIENTED_EDGE('',*,*,#2787,.F.);
#3609=ORIENTED_EDGE('',*,*,#2789,.F.);
#3610=ORIENTED_EDGE('',*,*,#2790,.F.);
#3611=ORIENTED_EDGE('',*,*,#2791,.T.);
#3612=ORIENTED_EDGE('',*,*,#2792,.F.);
#3613=ORIENTED_EDGE('',*,*,#2791,.F.);
#3614=ORIENTED_EDGE('',*,*,#2790,.T.);
#3615=ORIENTED_EDGE('',*,*,#2788,.T.);
#3616=ORIENTED_EDGE('',*,*,#2793,.F.);
#3617=ORIENTED_EDGE('',*,*,#2794,.F.);
#3618=ORIENTED_EDGE('',*,*,#2795,.T.);
#3619=ORIENTED_EDGE('',*,*,#2796,.F.);
#3620=ORIENTED_EDGE('',*,*,#2795,.F.);
#3621=ORIENTED_EDGE('',*,*,#2797,.F.);
#3622=ORIENTED_EDGE('',*,*,#2798,.F.);
#3623=ORIENTED_EDGE('',*,*,#2799,.T.);
#3624=ORIENTED_EDGE('',*,*,#2800,.F.);
#3625=ORIENTED_EDGE('',*,*,#2799,.F.);
#3626=ORIENTED_EDGE('',*,*,#2798,.T.);
#3627=ORIENTED_EDGE('',*,*,#2796,.T.);
#3628=ORIENTED_EDGE('',*,*,#2801,.F.);
#3629=ORIENTED_EDGE('',*,*,#2802,.F.);
#3630=ORIENTED_EDGE('',*,*,#2803,.T.);
#3631=ORIENTED_EDGE('',*,*,#2804,.F.);
#3632=ORIENTED_EDGE('',*,*,#2803,.F.);
#3633=ORIENTED_EDGE('',*,*,#2805,.F.);
#3634=ORIENTED_EDGE('',*,*,#2806,.F.);
#3635=ORIENTED_EDGE('',*,*,#2807,.T.);
#3636=ORIENTED_EDGE('',*,*,#2808,.F.);
#3637=ORIENTED_EDGE('',*,*,#2807,.F.);
#3638=ORIENTED_EDGE('',*,*,#2806,.T.);
#3639=ORIENTED_EDGE('',*,*,#2804,.T.);
#3640=ORIENTED_EDGE('',*,*,#2809,.F.);
#3641=ORIENTED_EDGE('',*,*,#2810,.F.);
#3642=ORIENTED_EDGE('',*,*,#2811,.T.);
#3643=ORIENTED_EDGE('',*,*,#2812,.F.);
#3644=ORIENTED_EDGE('',*,*,#2811,.F.);
#3645=ORIENTED_EDGE('',*,*,#2813,.F.);
#3646=ORIENTED_EDGE('',*,*,#2814,.F.);
#3647=ORIENTED_EDGE('',*,*,#2815,.T.);
#3648=ORIENTED_EDGE('',*,*,#2816,.F.);
#3649=ORIENTED_EDGE('',*,*,#2815,.F.);
#3650=ORIENTED_EDGE('',*,*,#2814,.T.);
#3651=ORIENTED_EDGE('',*,*,#2812,.T.);
#3652=ORIENTED_EDGE('',*,*,#2817,.F.);
#3653=ORIENTED_EDGE('',*,*,#2818,.T.);
#3654=ORIENTED_EDGE('',*,*,#2819,.T.);
#3655=ORIENTED_EDGE('',*,*,#2820,.F.);
#3656=ORIENTED_EDGE('',*,*,#2821,.F.);
#3657=ORIENTED_EDGE('',*,*,#2820,.T.);
#3658=ORIENTED_EDGE('',*,*,#2822,.T.);
#3659=ORIENTED_EDGE('',*,*,#2823,.F.);
#3660=ORIENTED_EDGE('',*,*,#2824,.T.);
#3661=ORIENTED_EDGE('',*,*,#2825,.F.);
#3662=ORIENTED_EDGE('',*,*,#2826,.F.);
#3663=ORIENTED_EDGE('',*,*,#2822,.F.);
#3664=ORIENTED_EDGE('',*,*,#2819,.F.);
#3665=ORIENTED_EDGE('',*,*,#2827,.F.);
#3666=ORIENTED_EDGE('',*,*,#2828,.F.);
#3667=ORIENTED_EDGE('',*,*,#2825,.T.);
#3668=ORIENTED_EDGE('',*,*,#2829,.T.);
#3669=ORIENTED_EDGE('',*,*,#2830,.F.);
#3670=ORIENTED_EDGE('',*,*,#2831,.F.);
#3671=ORIENTED_EDGE('',*,*,#2830,.T.);
#3672=ORIENTED_EDGE('',*,*,#2832,.T.);
#3673=ORIENTED_EDGE('',*,*,#2833,.F.);
#3674=ORIENTED_EDGE('',*,*,#2827,.T.);
#3675=ORIENTED_EDGE('',*,*,#2818,.F.);
#3676=ORIENTED_EDGE('',*,*,#2834,.F.);
#3677=ORIENTED_EDGE('',*,*,#2832,.F.);
#3678=ORIENTED_EDGE('',*,*,#2829,.F.);
#3679=ORIENTED_EDGE('',*,*,#2824,.F.);
#3680=ORIENTED_EDGE('',*,*,#2784,.T.);
#3681=ORIENTED_EDGE('',*,*,#2835,.T.);
#3682=ORIENTED_EDGE('',*,*,#2810,.T.);
#3683=ORIENTED_EDGE('',*,*,#2809,.T.);
#3684=ORIENTED_EDGE('',*,*,#2836,.T.);
#3685=ORIENTED_EDGE('',*,*,#2802,.T.);
#3686=ORIENTED_EDGE('',*,*,#2801,.T.);
#3687=ORIENTED_EDGE('',*,*,#2837,.T.);
#3688=ORIENTED_EDGE('',*,*,#2794,.T.);
#3689=ORIENTED_EDGE('',*,*,#2793,.T.);
#3690=ORIENTED_EDGE('',*,*,#2838,.T.);
#3691=ORIENTED_EDGE('',*,*,#2786,.T.);
#3692=ORIENTED_EDGE('',*,*,#2785,.T.);
#3693=ORIENTED_EDGE('',*,*,#2839,.T.);
#3694=ORIENTED_EDGE('',*,*,#2780,.T.);
#3695=ORIENTED_EDGE('',*,*,#2839,.F.);
#3696=ORIENTED_EDGE('',*,*,#2789,.T.);
#3697=ORIENTED_EDGE('',*,*,#2838,.F.);
#3698=ORIENTED_EDGE('',*,*,#2797,.T.);
#3699=ORIENTED_EDGE('',*,*,#2837,.F.);
#3700=ORIENTED_EDGE('',*,*,#2805,.T.);
#3701=ORIENTED_EDGE('',*,*,#2836,.F.);
#3702=ORIENTED_EDGE('',*,*,#2813,.T.);
#3703=ORIENTED_EDGE('',*,*,#2835,.F.);
#3704=ORIENTED_EDGE('',*,*,#2833,.T.);
#3705=ORIENTED_EDGE('',*,*,#2834,.T.);
#3706=ORIENTED_EDGE('',*,*,#2823,.T.);
#3707=ORIENTED_EDGE('',*,*,#2826,.T.);
#3708=ORIENTED_EDGE('',*,*,#2840,.T.);
#3709=ORIENTED_EDGE('',*,*,#2841,.T.);
#3710=ORIENTED_EDGE('',*,*,#2842,.F.);
#3711=ORIENTED_EDGE('',*,*,#2843,.F.);
#3712=ORIENTED_EDGE('',*,*,#2844,.T.);
#3713=ORIENTED_EDGE('',*,*,#2843,.T.);
#3714=ORIENTED_EDGE('',*,*,#2845,.F.);
#3715=ORIENTED_EDGE('',*,*,#2846,.F.);
#3716=ORIENTED_EDGE('',*,*,#2779,.T.);
#3717=ORIENTED_EDGE('',*,*,#2847,.T.);
#3718=ORIENTED_EDGE('',*,*,#2846,.T.);
#3719=ORIENTED_EDGE('',*,*,#2848,.F.);
#3720=ORIENTED_EDGE('',*,*,#2849,.F.);
#3721=ORIENTED_EDGE('',*,*,#2747,.T.);
#3722=ORIENTED_EDGE('',*,*,#2750,.T.);
#3723=ORIENTED_EDGE('',*,*,#2850,.T.);
#3724=ORIENTED_EDGE('',*,*,#2849,.T.);
#3725=ORIENTED_EDGE('',*,*,#2851,.F.);
#3726=ORIENTED_EDGE('',*,*,#2841,.F.);
#3727=ORIENTED_EDGE('',*,*,#2781,.T.);
#3728=ORIENTED_EDGE('',*,*,#2851,.T.);
#3729=ORIENTED_EDGE('',*,*,#2848,.T.);
#3730=ORIENTED_EDGE('',*,*,#2845,.T.);
#3731=ORIENTED_EDGE('',*,*,#2842,.T.);
#3732=ORIENTED_EDGE('',*,*,#2792,.T.);
#3733=ORIENTED_EDGE('',*,*,#2800,.T.);
#3734=ORIENTED_EDGE('',*,*,#2808,.T.);
#3735=ORIENTED_EDGE('',*,*,#2816,.T.);
#3736=ORIENTED_EDGE('',*,*,#2850,.F.);
#3737=ORIENTED_EDGE('',*,*,#2840,.F.);
#3738=ORIENTED_EDGE('',*,*,#2844,.F.);
#3739=ORIENTED_EDGE('',*,*,#2847,.F.);
#3740=ORIENTED_EDGE('',*,*,#2756,.T.);
#3741=ORIENTED_EDGE('',*,*,#2828,.T.);
#3742=ORIENTED_EDGE('',*,*,#2831,.T.);
#3743=ORIENTED_EDGE('',*,*,#2817,.T.);
#3744=ORIENTED_EDGE('',*,*,#2821,.T.);
#3745=ORIENTED_EDGE('',*,*,#2774,.T.);
#3746=ORIENTED_EDGE('',*,*,#2771,.T.);
#3747=ORIENTED_EDGE('',*,*,#2768,.T.);
#3748=ORIENTED_EDGE('',*,*,#2765,.T.);
#3749=ORIENTED_EDGE('',*,*,#2762,.T.);
#3750=ORIENTED_EDGE('',*,*,#2759,.T.);
#3751=ORIENTED_EDGE('',*,*,#2753,.T.);
#3752=ORIENTED_EDGE('',*,*,#2852,.F.);
#3753=ORIENTED_EDGE('',*,*,#2853,.T.);
#3754=ORIENTED_EDGE('',*,*,#2854,.T.);
#3755=ORIENTED_EDGE('',*,*,#2853,.F.);
#3756=ORIENTED_EDGE('',*,*,#2855,.F.);
#3757=ORIENTED_EDGE('',*,*,#2856,.T.);
#3758=ORIENTED_EDGE('',*,*,#2857,.T.);
#3759=ORIENTED_EDGE('',*,*,#2856,.F.);
#3760=ORIENTED_EDGE('',*,*,#2855,.T.);
#3761=ORIENTED_EDGE('',*,*,#2852,.T.);
#3762=ORIENTED_EDGE('',*,*,#2857,.F.);
#3763=ORIENTED_EDGE('',*,*,#2854,.F.);
#3764=ORIENTED_EDGE('',*,*,#2858,.F.);
#3765=ORIENTED_EDGE('',*,*,#2859,.T.);
#3766=ORIENTED_EDGE('',*,*,#2860,.T.);
#3767=ORIENTED_EDGE('',*,*,#2859,.F.);
#3768=ORIENTED_EDGE('',*,*,#2861,.F.);
#3769=ORIENTED_EDGE('',*,*,#2862,.T.);
#3770=ORIENTED_EDGE('',*,*,#2863,.T.);
#3771=ORIENTED_EDGE('',*,*,#2862,.F.);
#3772=ORIENTED_EDGE('',*,*,#2861,.T.);
#3773=ORIENTED_EDGE('',*,*,#2858,.T.);
#3774=ORIENTED_EDGE('',*,*,#2863,.F.);
#3775=ORIENTED_EDGE('',*,*,#2860,.F.);
#3776=ORIENTED_EDGE('',*,*,#2864,.F.);
#3777=ORIENTED_EDGE('',*,*,#2865,.T.);
#3778=ORIENTED_EDGE('',*,*,#2866,.T.);
#3779=ORIENTED_EDGE('',*,*,#2865,.F.);
#3780=ORIENTED_EDGE('',*,*,#2867,.F.);
#3781=ORIENTED_EDGE('',*,*,#2868,.T.);
#3782=ORIENTED_EDGE('',*,*,#2869,.T.);
#3783=ORIENTED_EDGE('',*,*,#2868,.F.);
#3784=ORIENTED_EDGE('',*,*,#2867,.T.);
#3785=ORIENTED_EDGE('',*,*,#2864,.T.);
#3786=ORIENTED_EDGE('',*,*,#2869,.F.);
#3787=ORIENTED_EDGE('',*,*,#2866,.F.);
#3788=ORIENTED_EDGE('',*,*,#2870,.F.);
#3789=ORIENTED_EDGE('',*,*,#2871,.T.);
#3790=ORIENTED_EDGE('',*,*,#2872,.T.);
#3791=ORIENTED_EDGE('',*,*,#2871,.F.);
#3792=ORIENTED_EDGE('',*,*,#2873,.F.);
#3793=ORIENTED_EDGE('',*,*,#2874,.T.);
#3794=ORIENTED_EDGE('',*,*,#2875,.T.);
#3795=ORIENTED_EDGE('',*,*,#2874,.F.);
#3796=ORIENTED_EDGE('',*,*,#2873,.T.);
#3797=ORIENTED_EDGE('',*,*,#2870,.T.);
#3798=ORIENTED_EDGE('',*,*,#2875,.F.);
#3799=ORIENTED_EDGE('',*,*,#2872,.F.);
#3800=ORIENTED_EDGE('',*,*,#2876,.F.);
#3801=ORIENTED_EDGE('',*,*,#2877,.F.);
#3802=ORIENTED_EDGE('',*,*,#2878,.F.);
#3803=ORIENTED_EDGE('',*,*,#2879,.F.);
#3804=ORIENTED_EDGE('',*,*,#2880,.F.);
#3805=ORIENTED_EDGE('',*,*,#2881,.F.);
#3806=ORIENTED_EDGE('',*,*,#2882,.T.);
#3807=ORIENTED_EDGE('',*,*,#2877,.T.);
#3808=ORIENTED_EDGE('',*,*,#2883,.T.);
#3809=ORIENTED_EDGE('',*,*,#2884,.F.);
#3810=ORIENTED_EDGE('',*,*,#2885,.F.);
#3811=ORIENTED_EDGE('',*,*,#2878,.T.);
#3812=ORIENTED_EDGE('',*,*,#2885,.T.);
#3813=ORIENTED_EDGE('',*,*,#2886,.F.);
#3814=ORIENTED_EDGE('',*,*,#2887,.F.);
#3815=ORIENTED_EDGE('',*,*,#2879,.T.);
#3816=ORIENTED_EDGE('',*,*,#2887,.T.);
#3817=ORIENTED_EDGE('',*,*,#2888,.F.);
#3818=ORIENTED_EDGE('',*,*,#2889,.F.);
#3819=ORIENTED_EDGE('',*,*,#2880,.T.);
#3820=ORIENTED_EDGE('',*,*,#2889,.T.);
#3821=ORIENTED_EDGE('',*,*,#2890,.F.);
#3822=ORIENTED_EDGE('',*,*,#2891,.F.);
#3823=ORIENTED_EDGE('',*,*,#2881,.T.);
#3824=ORIENTED_EDGE('',*,*,#2891,.T.);
#3825=ORIENTED_EDGE('',*,*,#2892,.F.);
#3826=ORIENTED_EDGE('',*,*,#2893,.F.);
#3827=ORIENTED_EDGE('',*,*,#2876,.T.);
#3828=ORIENTED_EDGE('',*,*,#2893,.T.);
#3829=ORIENTED_EDGE('',*,*,#2894,.F.);
#3830=ORIENTED_EDGE('',*,*,#2883,.F.);
#3831=ORIENTED_EDGE('',*,*,#2894,.T.);
#3832=ORIENTED_EDGE('',*,*,#2892,.T.);
#3833=ORIENTED_EDGE('',*,*,#2890,.T.);
#3834=ORIENTED_EDGE('',*,*,#2888,.T.);
#3835=ORIENTED_EDGE('',*,*,#2886,.T.);
#3836=ORIENTED_EDGE('',*,*,#2884,.T.);
#3837=ORIENTED_EDGE('',*,*,#2882,.F.);
#3838=ORIENTED_EDGE('',*,*,#2895,.T.);
#3839=ORIENTED_EDGE('',*,*,#2896,.T.);
#3840=ORIENTED_EDGE('',*,*,#2895,.F.);
#3841=ORIENTED_EDGE('',*,*,#2896,.F.);
#3842=ORIENTED_EDGE('',*,*,#2897,.F.);
#3843=ORIENTED_EDGE('',*,*,#2898,.T.);
#3844=ORIENTED_EDGE('',*,*,#2899,.T.);
#3845=ORIENTED_EDGE('',*,*,#2898,.F.);
#3846=ORIENTED_EDGE('',*,*,#2897,.T.);
#3847=ORIENTED_EDGE('',*,*,#2899,.F.);
#3848=ORIENTED_EDGE('',*,*,#2900,.F.);
#3849=ORIENTED_EDGE('',*,*,#2901,.T.);
#3850=ORIENTED_EDGE('',*,*,#2902,.T.);
#3851=ORIENTED_EDGE('',*,*,#2901,.F.);
#3852=ORIENTED_EDGE('',*,*,#2900,.T.);
#3853=ORIENTED_EDGE('',*,*,#2902,.F.);
#3854=ORIENTED_EDGE('',*,*,#2903,.F.);
#3855=ORIENTED_EDGE('',*,*,#2904,.T.);
#3856=ORIENTED_EDGE('',*,*,#2905,.F.);
#3857=ORIENTED_EDGE('',*,*,#2904,.F.);
#3858=ORIENTED_EDGE('',*,*,#2906,.F.);
#3859=ORIENTED_EDGE('',*,*,#2907,.T.);
#3860=ORIENTED_EDGE('',*,*,#2908,.F.);
#3861=ORIENTED_EDGE('',*,*,#2907,.F.);
#3862=ORIENTED_EDGE('',*,*,#2909,.T.);
#3863=ORIENTED_EDGE('',*,*,#2910,.T.);
#3864=ORIENTED_EDGE('',*,*,#2911,.F.);
#3865=ORIENTED_EDGE('',*,*,#2912,.F.);
#3866=ORIENTED_EDGE('',*,*,#2905,.T.);
#3867=ORIENTED_EDGE('',*,*,#2908,.T.);
#3868=ORIENTED_EDGE('',*,*,#2913,.T.);
#3869=ORIENTED_EDGE('',*,*,#2912,.T.);
#3870=ORIENTED_EDGE('',*,*,#2914,.F.);
#3871=ORIENTED_EDGE('',*,*,#2915,.F.);
#3872=ORIENTED_EDGE('',*,*,#2916,.T.);
#3873=ORIENTED_EDGE('',*,*,#2915,.T.);
#3874=ORIENTED_EDGE('',*,*,#2917,.F.);
#3875=ORIENTED_EDGE('',*,*,#2918,.F.);
#3876=ORIENTED_EDGE('',*,*,#2903,.T.);
#3877=ORIENTED_EDGE('',*,*,#2906,.T.);
#3878=ORIENTED_EDGE('',*,*,#2919,.T.);
#3879=ORIENTED_EDGE('',*,*,#2918,.T.);
#3880=ORIENTED_EDGE('',*,*,#2920,.F.);
#3881=ORIENTED_EDGE('',*,*,#2910,.F.);
#3882=ORIENTED_EDGE('',*,*,#2920,.T.);
#3883=ORIENTED_EDGE('',*,*,#2917,.T.);
#3884=ORIENTED_EDGE('',*,*,#2914,.T.);
#3885=ORIENTED_EDGE('',*,*,#2911,.T.);
#3886=ORIENTED_EDGE('',*,*,#2919,.F.);
#3887=ORIENTED_EDGE('',*,*,#2909,.F.);
#3888=ORIENTED_EDGE('',*,*,#2913,.F.);
#3889=ORIENTED_EDGE('',*,*,#2916,.F.);
#3890=ORIENTED_EDGE('',*,*,#2921,.T.);
#3891=ORIENTED_EDGE('',*,*,#2922,.T.);
#3892=ORIENTED_EDGE('',*,*,#2923,.T.);
#3893=ORIENTED_EDGE('',*,*,#2924,.F.);
#3894=ORIENTED_EDGE('',*,*,#2925,.T.);
#3895=ORIENTED_EDGE('',*,*,#2926,.T.);
#3896=ORIENTED_EDGE('',*,*,#2927,.T.);
#3897=ORIENTED_EDGE('',*,*,#2922,.F.);
#3898=ORIENTED_EDGE('',*,*,#2928,.T.);
#3899=ORIENTED_EDGE('',*,*,#2929,.T.);
#3900=ORIENTED_EDGE('',*,*,#2930,.T.);
#3901=ORIENTED_EDGE('',*,*,#2926,.F.);
#3902=ORIENTED_EDGE('',*,*,#2931,.T.);
#3903=ORIENTED_EDGE('',*,*,#2932,.T.);
#3904=ORIENTED_EDGE('',*,*,#2933,.T.);
#3905=ORIENTED_EDGE('',*,*,#2929,.F.);
#3906=ORIENTED_EDGE('',*,*,#2934,.T.);
#3907=ORIENTED_EDGE('',*,*,#2935,.T.);
#3908=ORIENTED_EDGE('',*,*,#2936,.T.);
#3909=ORIENTED_EDGE('',*,*,#2932,.F.);
#3910=ORIENTED_EDGE('',*,*,#2937,.T.);
#3911=ORIENTED_EDGE('',*,*,#2924,.T.);
#3912=ORIENTED_EDGE('',*,*,#2938,.T.);
#3913=ORIENTED_EDGE('',*,*,#2935,.F.);
#3914=ORIENTED_EDGE('',*,*,#2937,.F.);
#3915=ORIENTED_EDGE('',*,*,#2934,.F.);
#3916=ORIENTED_EDGE('',*,*,#2931,.F.);
#3917=ORIENTED_EDGE('',*,*,#2928,.F.);
#3918=ORIENTED_EDGE('',*,*,#2925,.F.);
#3919=ORIENTED_EDGE('',*,*,#2921,.F.);
#3920=ORIENTED_EDGE('',*,*,#2938,.F.);
#3921=ORIENTED_EDGE('',*,*,#2923,.F.);
#3922=ORIENTED_EDGE('',*,*,#2927,.F.);
#3923=ORIENTED_EDGE('',*,*,#2930,.F.);
#3924=ORIENTED_EDGE('',*,*,#2933,.F.);
#3925=ORIENTED_EDGE('',*,*,#2936,.F.);
#3926=ORIENTED_EDGE('',*,*,#2939,.F.);
#3927=ORIENTED_EDGE('',*,*,#2940,.F.);
#3928=ORIENTED_EDGE('',*,*,#2941,.F.);
#3929=ORIENTED_EDGE('',*,*,#2942,.T.);
#3930=ORIENTED_EDGE('',*,*,#2940,.T.);
#3931=ORIENTED_EDGE('',*,*,#2942,.F.);
#3932=ORIENTED_EDGE('',*,*,#2943,.F.);
#3933=ORIENTED_EDGE('',*,*,#2944,.T.);
#3934=ORIENTED_EDGE('',*,*,#2941,.T.);
#3935=ORIENTED_EDGE('',*,*,#2944,.F.);
#3936=ORIENTED_EDGE('',*,*,#2945,.F.);
#3937=ORIENTED_EDGE('',*,*,#2946,.T.);
#3938=ORIENTED_EDGE('',*,*,#2943,.T.);
#3939=ORIENTED_EDGE('',*,*,#2946,.F.);
#3940=ORIENTED_EDGE('',*,*,#2945,.T.);
#3941=ORIENTED_EDGE('',*,*,#2947,.F.);
#3942=ORIENTED_EDGE('',*,*,#2948,.F.);
#3943=ORIENTED_EDGE('',*,*,#2949,.T.);
#3944=ORIENTED_EDGE('',*,*,#2947,.T.);
#3945=ORIENTED_EDGE('',*,*,#2949,.F.);
#3946=ORIENTED_EDGE('',*,*,#2939,.T.);
#3947=ORIENTED_EDGE('',*,*,#2950,.T.);
#3948=ORIENTED_EDGE('',*,*,#2948,.T.);
#3949=ORIENTED_EDGE('',*,*,#2950,.F.);
#3950=ORIENTED_EDGE('',*,*,#2951,.F.);
#3951=ORIENTED_EDGE('',*,*,#2952,.T.);
#3952=ORIENTED_EDGE('',*,*,#2953,.F.);
#3953=ORIENTED_EDGE('',*,*,#2952,.F.);
#3954=ORIENTED_EDGE('',*,*,#2951,.T.);
#3955=ORIENTED_EDGE('',*,*,#2954,.F.);
#3956=ORIENTED_EDGE('',*,*,#2955,.T.);
#3957=ORIENTED_EDGE('',*,*,#2956,.T.);
#3958=ORIENTED_EDGE('',*,*,#2957,.T.);
#3959=ORIENTED_EDGE('',*,*,#2958,.T.);
#3960=ORIENTED_EDGE('',*,*,#2959,.T.);
#3961=ORIENTED_EDGE('',*,*,#2960,.T.);
#3962=ORIENTED_EDGE('',*,*,#2961,.T.);
#3963=ORIENTED_EDGE('',*,*,#2962,.F.);
#3964=ORIENTED_EDGE('',*,*,#2963,.F.);
#3965=ORIENTED_EDGE('',*,*,#2964,.F.);
#3966=ORIENTED_EDGE('',*,*,#2965,.F.);
#3967=ORIENTED_EDGE('',*,*,#2966,.F.);
#3968=ORIENTED_EDGE('',*,*,#2967,.F.);
#3969=ORIENTED_EDGE('',*,*,#2968,.F.);
#3970=ORIENTED_EDGE('',*,*,#2963,.T.);
#3971=ORIENTED_EDGE('',*,*,#2969,.T.);
#3972=ORIENTED_EDGE('',*,*,#2960,.F.);
#3973=ORIENTED_EDGE('',*,*,#2970,.F.);
#3974=ORIENTED_EDGE('',*,*,#2964,.T.);
#3975=ORIENTED_EDGE('',*,*,#2970,.T.);
#3976=ORIENTED_EDGE('',*,*,#2959,.F.);
#3977=ORIENTED_EDGE('',*,*,#2971,.F.);
#3978=ORIENTED_EDGE('',*,*,#2965,.T.);
#3979=ORIENTED_EDGE('',*,*,#2971,.T.);
#3980=ORIENTED_EDGE('',*,*,#2958,.F.);
#3981=ORIENTED_EDGE('',*,*,#2972,.F.);
#3982=ORIENTED_EDGE('',*,*,#2966,.T.);
#3983=ORIENTED_EDGE('',*,*,#2972,.T.);
#3984=ORIENTED_EDGE('',*,*,#2957,.F.);
#3985=ORIENTED_EDGE('',*,*,#2973,.F.);
#3986=ORIENTED_EDGE('',*,*,#2967,.T.);
#3987=ORIENTED_EDGE('',*,*,#2973,.T.);
#3988=ORIENTED_EDGE('',*,*,#2956,.F.);
#3989=ORIENTED_EDGE('',*,*,#2974,.F.);
#3990=ORIENTED_EDGE('',*,*,#2962,.T.);
#3991=ORIENTED_EDGE('',*,*,#2974,.T.);
#3992=ORIENTED_EDGE('',*,*,#2955,.F.);
#3993=ORIENTED_EDGE('',*,*,#2969,.F.);
#3994=ORIENTED_EDGE('',*,*,#2975,.F.);
#3995=ORIENTED_EDGE('',*,*,#2953,.T.);
#3996=ORIENTED_EDGE('',*,*,#2975,.T.);
#3997=ORIENTED_EDGE('',*,*,#2976,.T.);
#3998=ORIENTED_EDGE('',*,*,#2977,.F.);
#3999=ORIENTED_EDGE('',*,*,#2976,.F.);
#4000=ORIENTED_EDGE('',*,*,#2978,.F.);
#4001=ORIENTED_EDGE('',*,*,#2977,.T.);
#4002=ORIENTED_EDGE('',*,*,#2961,.F.);
#4003=ORIENTED_EDGE('',*,*,#2979,.T.);
#4004=ORIENTED_EDGE('',*,*,#2978,.T.);
#4005=ORIENTED_EDGE('',*,*,#2979,.F.);
#4006=ORIENTED_EDGE('',*,*,#2980,.F.);
#4007=ORIENTED_EDGE('',*,*,#2981,.T.);
#4008=ORIENTED_EDGE('',*,*,#2968,.T.);
#4009=ORIENTED_EDGE('',*,*,#2981,.F.);
#4010=ORIENTED_EDGE('',*,*,#2980,.T.);
#4011=ORIENTED_EDGE('',*,*,#2982,.F.);
#4012=ORIENTED_EDGE('',*,*,#2982,.T.);
#4013=ORIENTED_EDGE('',*,*,#2983,.T.);
#4014=ORIENTED_EDGE('',*,*,#2954,.T.);
#4015=ORIENTED_EDGE('',*,*,#2983,.F.);
#4016=ORIENTED_EDGE('',*,*,#2984,.F.);
#4017=ORIENTED_EDGE('',*,*,#2985,.T.);
#4018=ORIENTED_EDGE('',*,*,#2986,.F.);
#4019=ORIENTED_EDGE('',*,*,#2987,.T.);
#4020=ORIENTED_EDGE('',*,*,#2984,.T.);
#4021=ORIENTED_EDGE('',*,*,#2987,.F.);
#4022=ORIENTED_EDGE('',*,*,#2986,.T.);
#4023=ORIENTED_EDGE('',*,*,#2988,.F.);
#4024=ORIENTED_EDGE('',*,*,#2989,.F.);
#4025=ORIENTED_EDGE('',*,*,#2990,.T.);
#4026=ORIENTED_EDGE('',*,*,#2988,.T.);
#4027=ORIENTED_EDGE('',*,*,#2990,.F.);
#4028=ORIENTED_EDGE('',*,*,#2989,.T.);
#4029=ORIENTED_EDGE('',*,*,#2991,.F.);
#4030=ORIENTED_EDGE('',*,*,#2991,.T.);
#4031=ORIENTED_EDGE('',*,*,#2992,.T.);
#4032=ORIENTED_EDGE('',*,*,#2985,.F.);
#4033=ORIENTED_EDGE('',*,*,#2992,.F.);
#4034=ORIENTED_EDGE('',*,*,#2993,.T.);
#4035=ORIENTED_EDGE('',*,*,#2994,.T.);
#4036=ORIENTED_EDGE('',*,*,#2995,.T.);
#4037=ORIENTED_EDGE('',*,*,#2996,.T.);
#4038=ORIENTED_EDGE('',*,*,#2997,.T.);
#4039=ORIENTED_EDGE('',*,*,#2998,.T.);
#4040=ORIENTED_EDGE('',*,*,#2999,.F.);
#4041=ORIENTED_EDGE('',*,*,#3000,.T.);
#4042=ORIENTED_EDGE('',*,*,#3001,.T.);
#4043=ORIENTED_EDGE('',*,*,#3002,.T.);
#4044=ORIENTED_EDGE('',*,*,#3003,.T.);
#4045=ORIENTED_EDGE('',*,*,#3004,.T.);
#4046=ORIENTED_EDGE('',*,*,#3005,.T.);
#4047=ORIENTED_EDGE('',*,*,#3006,.F.);
#4048=ORIENTED_EDGE('',*,*,#3007,.F.);
#4049=ORIENTED_EDGE('',*,*,#3005,.F.);
#4050=ORIENTED_EDGE('',*,*,#3008,.F.);
#4051=ORIENTED_EDGE('',*,*,#2994,.F.);
#4052=ORIENTED_EDGE('',*,*,#3008,.T.);
#4053=ORIENTED_EDGE('',*,*,#3004,.F.);
#4054=ORIENTED_EDGE('',*,*,#3009,.F.);
#4055=ORIENTED_EDGE('',*,*,#2995,.F.);
#4056=ORIENTED_EDGE('',*,*,#3009,.T.);
#4057=ORIENTED_EDGE('',*,*,#3003,.F.);
#4058=ORIENTED_EDGE('',*,*,#3010,.F.);
#4059=ORIENTED_EDGE('',*,*,#2996,.F.);
#4060=ORIENTED_EDGE('',*,*,#3010,.T.);
#4061=ORIENTED_EDGE('',*,*,#3002,.F.);
#4062=ORIENTED_EDGE('',*,*,#3011,.F.);
#4063=ORIENTED_EDGE('',*,*,#2997,.F.);
#4064=ORIENTED_EDGE('',*,*,#3011,.T.);
#4065=ORIENTED_EDGE('',*,*,#3001,.F.);
#4066=ORIENTED_EDGE('',*,*,#3012,.F.);
#4067=ORIENTED_EDGE('',*,*,#2998,.F.);
#4068=ORIENTED_EDGE('',*,*,#3012,.T.);
#4069=ORIENTED_EDGE('',*,*,#3000,.F.);
#4070=ORIENTED_EDGE('',*,*,#3007,.T.);
#4071=ORIENTED_EDGE('',*,*,#2993,.F.);
#4072=ORIENTED_EDGE('',*,*,#3006,.T.);
#4073=ORIENTED_EDGE('',*,*,#3013,.T.);
#4074=ORIENTED_EDGE('',*,*,#3014,.T.);
#4075=ORIENTED_EDGE('',*,*,#3013,.F.);
#4076=ORIENTED_EDGE('',*,*,#3015,.F.);
#4077=ORIENTED_EDGE('',*,*,#3016,.T.);
#4078=ORIENTED_EDGE('',*,*,#3014,.F.);
#4079=ORIENTED_EDGE('',*,*,#3017,.T.);
#4080=ORIENTED_EDGE('',*,*,#3015,.T.);
#4081=ORIENTED_EDGE('',*,*,#3017,.F.);
#4082=ORIENTED_EDGE('',*,*,#3018,.F.);
#4083=ORIENTED_EDGE('',*,*,#3019,.T.);
#4084=ORIENTED_EDGE('',*,*,#2999,.T.);
#4085=ORIENTED_EDGE('',*,*,#3019,.F.);
#4086=ORIENTED_EDGE('',*,*,#3020,.F.);
#4087=ORIENTED_EDGE('',*,*,#3021,.T.);
#4088=ORIENTED_EDGE('',*,*,#3018,.T.);
#4089=ORIENTED_EDGE('',*,*,#3021,.F.);
#4090=ORIENTED_EDGE('',*,*,#3020,.T.);
#4091=ORIENTED_EDGE('',*,*,#3022,.F.);
#4092=ORIENTED_EDGE('',*,*,#3022,.T.);
#4093=ORIENTED_EDGE('',*,*,#3023,.T.);
#4094=ORIENTED_EDGE('',*,*,#3016,.F.);
#4095=ORIENTED_EDGE('',*,*,#3023,.F.);
#4096=ORIENTED_EDGE('',*,*,#3024,.F.);
#4097=ORIENTED_EDGE('',*,*,#3025,.F.);
#4098=ORIENTED_EDGE('',*,*,#3026,.T.);
#4099=ORIENTED_EDGE('',*,*,#3024,.T.);
#4100=ORIENTED_EDGE('',*,*,#3026,.F.);
#4101=ORIENTED_EDGE('',*,*,#3027,.F.);
#4102=ORIENTED_EDGE('',*,*,#3028,.T.);
#4103=ORIENTED_EDGE('',*,*,#3025,.T.);
#4104=ORIENTED_EDGE('',*,*,#3028,.F.);
#4105=ORIENTED_EDGE('',*,*,#3029,.F.);
#4106=ORIENTED_EDGE('',*,*,#3030,.T.);
#4107=ORIENTED_EDGE('',*,*,#3027,.T.);
#4108=ORIENTED_EDGE('',*,*,#3030,.F.);
#4109=ORIENTED_EDGE('',*,*,#3029,.T.);
#4110=ORIENTED_EDGE('',*,*,#3031,.F.);
#4111=ORIENTED_EDGE('',*,*,#3032,.F.);
#4112=ORIENTED_EDGE('',*,*,#3033,.T.);
#4113=ORIENTED_EDGE('',*,*,#3031,.T.);
#4114=ORIENTED_EDGE('',*,*,#3033,.F.);
#4115=ORIENTED_EDGE('',*,*,#3034,.F.);
#4116=ORIENTED_EDGE('',*,*,#3035,.T.);
#4117=ORIENTED_EDGE('',*,*,#3032,.T.);
#4118=ORIENTED_EDGE('',*,*,#3035,.F.);
#4119=ORIENTED_EDGE('',*,*,#3036,.F.);
#4120=ORIENTED_EDGE('',*,*,#3037,.T.);
#4121=ORIENTED_EDGE('',*,*,#3034,.T.);
#4122=ORIENTED_EDGE('',*,*,#3037,.F.);
#4123=ORIENTED_EDGE('',*,*,#3036,.T.);
#4124=ORIENTED_EDGE('',*,*,#3038,.T.);
#4125=ORIENTED_EDGE('',*,*,#3039,.T.);
#4126=ORIENTED_EDGE('',*,*,#3040,.T.);
#4127=ORIENTED_EDGE('',*,*,#3041,.F.);
#4128=ORIENTED_EDGE('',*,*,#3042,.T.);
#4129=ORIENTED_EDGE('',*,*,#3043,.T.);
#4130=ORIENTED_EDGE('',*,*,#3044,.T.);
#4131=ORIENTED_EDGE('',*,*,#3039,.F.);
#4132=ORIENTED_EDGE('',*,*,#3045,.T.);
#4133=ORIENTED_EDGE('',*,*,#3046,.T.);
#4134=ORIENTED_EDGE('',*,*,#3047,.T.);
#4135=ORIENTED_EDGE('',*,*,#3043,.F.);
#4136=ORIENTED_EDGE('',*,*,#3048,.T.);
#4137=ORIENTED_EDGE('',*,*,#3049,.T.);
#4138=ORIENTED_EDGE('',*,*,#3050,.T.);
#4139=ORIENTED_EDGE('',*,*,#3046,.F.);
#4140=ORIENTED_EDGE('',*,*,#3051,.T.);
#4141=ORIENTED_EDGE('',*,*,#3052,.T.);
#4142=ORIENTED_EDGE('',*,*,#3053,.T.);
#4143=ORIENTED_EDGE('',*,*,#3049,.F.);
#4144=ORIENTED_EDGE('',*,*,#3054,.T.);
#4145=ORIENTED_EDGE('',*,*,#3041,.T.);
#4146=ORIENTED_EDGE('',*,*,#3055,.T.);
#4147=ORIENTED_EDGE('',*,*,#3052,.F.);
#4148=ORIENTED_EDGE('',*,*,#3054,.F.);
#4149=ORIENTED_EDGE('',*,*,#3051,.F.);
#4150=ORIENTED_EDGE('',*,*,#3048,.F.);
#4151=ORIENTED_EDGE('',*,*,#3045,.F.);
#4152=ORIENTED_EDGE('',*,*,#3042,.F.);
#4153=ORIENTED_EDGE('',*,*,#3038,.F.);
#4154=ORIENTED_EDGE('',*,*,#3055,.F.);
#4155=ORIENTED_EDGE('',*,*,#3040,.F.);
#4156=ORIENTED_EDGE('',*,*,#3044,.F.);
#4157=ORIENTED_EDGE('',*,*,#3047,.F.);
#4158=ORIENTED_EDGE('',*,*,#3050,.F.);
#4159=ORIENTED_EDGE('',*,*,#3053,.F.);
#4160=ORIENTED_EDGE('',*,*,#3056,.T.);
#4161=ORIENTED_EDGE('',*,*,#3057,.T.);
#4162=ORIENTED_EDGE('',*,*,#3058,.T.);
#4163=ORIENTED_EDGE('',*,*,#3059,.F.);
#4164=ORIENTED_EDGE('',*,*,#3060,.T.);
#4165=ORIENTED_EDGE('',*,*,#3061,.T.);
#4166=ORIENTED_EDGE('',*,*,#3062,.T.);
#4167=ORIENTED_EDGE('',*,*,#3057,.F.);
#4168=ORIENTED_EDGE('',*,*,#3063,.T.);
#4169=ORIENTED_EDGE('',*,*,#3064,.T.);
#4170=ORIENTED_EDGE('',*,*,#3065,.T.);
#4171=ORIENTED_EDGE('',*,*,#3061,.F.);
#4172=ORIENTED_EDGE('',*,*,#3066,.T.);
#4173=ORIENTED_EDGE('',*,*,#3067,.T.);
#4174=ORIENTED_EDGE('',*,*,#3068,.T.);
#4175=ORIENTED_EDGE('',*,*,#3064,.F.);
#4176=ORIENTED_EDGE('',*,*,#3069,.T.);
#4177=ORIENTED_EDGE('',*,*,#3070,.T.);
#4178=ORIENTED_EDGE('',*,*,#3071,.T.);
#4179=ORIENTED_EDGE('',*,*,#3067,.F.);
#4180=ORIENTED_EDGE('',*,*,#3072,.T.);
#4181=ORIENTED_EDGE('',*,*,#3059,.T.);
#4182=ORIENTED_EDGE('',*,*,#3073,.T.);
#4183=ORIENTED_EDGE('',*,*,#3070,.F.);
#4184=ORIENTED_EDGE('',*,*,#3072,.F.);
#4185=ORIENTED_EDGE('',*,*,#3069,.F.);
#4186=ORIENTED_EDGE('',*,*,#3066,.F.);
#4187=ORIENTED_EDGE('',*,*,#3063,.F.);
#4188=ORIENTED_EDGE('',*,*,#3060,.F.);
#4189=ORIENTED_EDGE('',*,*,#3056,.F.);
#4190=ORIENTED_EDGE('',*,*,#3073,.F.);
#4191=ORIENTED_EDGE('',*,*,#3058,.F.);
#4192=ORIENTED_EDGE('',*,*,#3062,.F.);
#4193=ORIENTED_EDGE('',*,*,#3065,.F.);
#4194=ORIENTED_EDGE('',*,*,#3068,.F.);
#4195=ORIENTED_EDGE('',*,*,#3071,.F.);
#4196=ORIENTED_EDGE('',*,*,#3074,.F.);
#4197=ORIENTED_EDGE('',*,*,#3075,.F.);
#4198=ORIENTED_EDGE('',*,*,#3076,.F.);
#4199=ORIENTED_EDGE('',*,*,#3077,.T.);
#4200=ORIENTED_EDGE('',*,*,#3075,.T.);
#4201=ORIENTED_EDGE('',*,*,#3077,.F.);
#4202=ORIENTED_EDGE('',*,*,#3078,.F.);
#4203=ORIENTED_EDGE('',*,*,#3079,.T.);
#4204=ORIENTED_EDGE('',*,*,#3076,.T.);
#4205=ORIENTED_EDGE('',*,*,#3079,.F.);
#4206=ORIENTED_EDGE('',*,*,#3080,.F.);
#4207=ORIENTED_EDGE('',*,*,#3081,.T.);
#4208=ORIENTED_EDGE('',*,*,#3078,.T.);
#4209=ORIENTED_EDGE('',*,*,#3081,.F.);
#4210=ORIENTED_EDGE('',*,*,#3080,.T.);
#4211=ORIENTED_EDGE('',*,*,#3082,.F.);
#4212=ORIENTED_EDGE('',*,*,#3083,.F.);
#4213=ORIENTED_EDGE('',*,*,#3084,.T.);
#4214=ORIENTED_EDGE('',*,*,#3082,.T.);
#4215=ORIENTED_EDGE('',*,*,#3084,.F.);
#4216=ORIENTED_EDGE('',*,*,#3074,.T.);
#4217=ORIENTED_EDGE('',*,*,#3085,.T.);
#4218=ORIENTED_EDGE('',*,*,#3083,.T.);
#4219=ORIENTED_EDGE('',*,*,#3085,.F.);
#4220=CYLINDRICAL_SURFACE('',#4851,0.5);
#4221=CYLINDRICAL_SURFACE('',#4855,0.5);
#4222=CYLINDRICAL_SURFACE('',#4859,0.5);
#4223=CYLINDRICAL_SURFACE('',#4863,0.5);
#4224=CYLINDRICAL_SURFACE('',#4867,0.21);
#4225=CYLINDRICAL_SURFACE('',#4870,0.21);
#4226=CYLINDRICAL_SURFACE('',#4873,0.21);
#4227=CYLINDRICAL_SURFACE('',#4876,0.21);
#4228=CYLINDRICAL_SURFACE('',#4903,0.45);
#4229=CYLINDRICAL_SURFACE('',#4908,0.45);
#4230=CYLINDRICAL_SURFACE('',#4910,0.275);
#4231=CYLINDRICAL_SURFACE('',#4914,0.275);
#4232=CYLINDRICAL_SURFACE('',#4918,0.275);
#4233=CYLINDRICAL_SURFACE('',#4921,0.275);
#4234=CYLINDRICAL_SURFACE('',#4934,0.45);
#4235=CYLINDRICAL_SURFACE('',#4939,0.45);
#4236=CYLINDRICAL_SURFACE('',#4941,0.275);
#4237=CYLINDRICAL_SURFACE('',#4945,0.275);
#4238=CYLINDRICAL_SURFACE('',#4949,0.275);
#4239=CYLINDRICAL_SURFACE('',#4952,0.275);
#4240=CYLINDRICAL_SURFACE('',#4962,0.15);
#4241=CYLINDRICAL_SURFACE('',#4965,0.15);
#4242=CYLINDRICAL_SURFACE('',#4968,0.225);
#4243=CYLINDRICAL_SURFACE('',#4971,0.225);
#4244=CYLINDRICAL_SURFACE('',#4974,0.225);
#4245=CYLINDRICAL_SURFACE('',#4977,0.225);
#4246=CYLINDRICAL_SURFACE('',#4980,0.225);
#4247=CYLINDRICAL_SURFACE('',#4983,0.225);
#4248=CYLINDRICAL_SURFACE('',#4986,0.21);
#4249=CYLINDRICAL_SURFACE('',#4989,0.21);
#4250=CYLINDRICAL_SURFACE('',#4992,0.21);
#4251=CYLINDRICAL_SURFACE('',#4995,0.21);
#4252=CYLINDRICAL_SURFACE('',#5005,0.15);
#4253=CYLINDRICAL_SURFACE('',#5008,0.15);
#4254=CYLINDRICAL_SURFACE('',#5011,0.225);
#4255=CYLINDRICAL_SURFACE('',#5014,0.225);
#4256=CYLINDRICAL_SURFACE('',#5017,0.225);
#4257=CYLINDRICAL_SURFACE('',#5020,0.225);
#4258=CYLINDRICAL_SURFACE('',#5023,0.225);
#4259=CYLINDRICAL_SURFACE('',#5026,0.225);
#4260=CYLINDRICAL_SURFACE('',#5040,0.165);
#4261=CYLINDRICAL_SURFACE('',#5044,0.165);
#4262=CYLINDRICAL_SURFACE('',#5048,0.15);
#4263=CYLINDRICAL_SURFACE('',#5052,0.15);
#4264=CYLINDRICAL_SURFACE('',#5056,0.165);
#4265=CYLINDRICAL_SURFACE('',#5060,0.165);
#4266=CYLINDRICAL_SURFACE('',#5064,0.165);
#4267=CYLINDRICAL_SURFACE('',#5068,0.165);
#4268=CYLINDRICAL_SURFACE('',#5072,0.165);
#4269=CYLINDRICAL_SURFACE('',#5076,0.165);
#4270=CYLINDRICAL_SURFACE('',#5080,0.685);
#4271=CYLINDRICAL_SURFACE('',#5085,0.685);
#4272=CYLINDRICAL_SURFACE('',#5090,0.2);
#4273=CYLINDRICAL_SURFACE('',#5092,0.515);
#4274=CYLINDRICAL_SURFACE('',#5096,0.2);
#4275=CYLINDRICAL_SURFACE('',#5098,0.515);
#4276=CYLINDRICAL_SURFACE('',#5102,0.2);
#4277=CYLINDRICAL_SURFACE('',#5104,0.515);
#4278=CYLINDRICAL_SURFACE('',#5108,0.2);
#4279=CYLINDRICAL_SURFACE('',#5110,0.515);
#4280=CYLINDRICAL_SURFACE('',#5122,0.3);
#4281=CYLINDRICAL_SURFACE('',#5130,0.2);
#4282=CYLINDRICAL_SURFACE('',#5133,0.3);
#4283=CYLINDRICAL_SURFACE('',#5139,0.2);
#4284=CYLINDRICAL_SURFACE('',#5142,0.3);
#4285=CYLINDRICAL_SURFACE('',#5148,0.2);
#4286=CYLINDRICAL_SURFACE('',#5151,0.3);
#4287=CYLINDRICAL_SURFACE('',#5157,0.2);
#4288=CYLINDRICAL_SURFACE('',#5160,0.3);
#4289=CYLINDRICAL_SURFACE('',#5175,0.685);
#4290=CYLINDRICAL_SURFACE('',#5179,0.15);
#4291=CYLINDRICAL_SURFACE('',#5185,0.15);
#4292=CYLINDRICAL_SURFACE('',#5191,0.225);
#4293=CYLINDRICAL_SURFACE('',#5194,0.225);
#4294=CYLINDRICAL_SURFACE('',#5218,0.425);
#4295=CYLINDRICAL_SURFACE('',#5226,0.24505);
#4296=CYLINDRICAL_SURFACE('',#5229,0.43);
#4297=CYLINDRICAL_SURFACE('',#5246,0.46);
#4298=CYLINDRICAL_SURFACE('',#5250,0.525);
#4299=CYLINDRICAL_SURFACE('',#5251,0.515);
#4300=CYLINDRICAL_SURFACE('',#5255,0.2);
#4301=CYLINDRICAL_SURFACE('',#5260,0.475);
#4302=CYLINDRICAL_SURFACE('',#5264,0.355);
#4303=CYLINDRICAL_SURFACE('',#5268,0.31);
#4304=CYLINDRICAL_SURFACE('',#5282,0.685);
#4305=CYLINDRICAL_SURFACE('',#5288,0.685);
#4306=CYLINDRICAL_SURFACE('',#5294,0.46);
#4307=CYLINDRICAL_SURFACE('',#5300,0.35);
#4308=CYLINDRICAL_SURFACE('',#5308,0.1954);
#4309=CYLINDRICAL_SURFACE('',#5336,0.35);
#4310=CYLINDRICAL_SURFACE('',#5344,0.1954);
#4311=ADVANCED_FACE('',(#572),#4220,.F.);
#4312=ADVANCED_FACE('',(#573),#405,.T.);
#4313=ADVANCED_FACE('',(#574),#4221,.F.);
#4314=ADVANCED_FACE('',(#575),#406,.T.);
#4315=ADVANCED_FACE('',(#576),#4222,.F.);
#4316=ADVANCED_FACE('',(#577),#407,.T.);
#4317=ADVANCED_FACE('',(#578),#4223,.F.);
#4318=ADVANCED_FACE('',(#579),#408,.T.);
#4319=ADVANCED_FACE('',(#580),#4224,.F.);
#4320=ADVANCED_FACE('',(#581),#4225,.F.);
#4321=ADVANCED_FACE('',(#582),#4226,.F.);
#4322=ADVANCED_FACE('',(#583),#4227,.F.);
#4323=ADVANCED_FACE('',(#584),#409,.T.);
#4324=ADVANCED_FACE('',(#585),#410,.T.);
#4325=ADVANCED_FACE('',(#586),#411,.T.);
#4326=ADVANCED_FACE('',(#587),#412,.T.);
#4327=ADVANCED_FACE('',(#588,#282,#283,#284,#285,#286,#287,#288,#289),#413,
 .T.);
#4328=ADVANCED_FACE('',(#589,#290,#291,#292,#293),#414,.F.);
#4329=ADVANCED_FACE('',(#590),#415,.T.);
#4330=ADVANCED_FACE('',(#591),#416,.T.);
#4331=ADVANCED_FACE('',(#592),#417,.T.);
#4332=ADVANCED_FACE('',(#593),#418,.T.);
#4333=ADVANCED_FACE('',(#594),#419,.T.);
#4334=ADVANCED_FACE('',(#595),#420,.F.);
#4335=ADVANCED_FACE('',(#596),#421,.T.);
#4336=ADVANCED_FACE('',(#597),#422,.T.);
#4337=ADVANCED_FACE('',(#598),#423,.T.);
#4338=ADVANCED_FACE('',(#599),#424,.T.);
#4339=ADVANCED_FACE('',(#600),#425,.T.);
#4340=ADVANCED_FACE('',(#601),#426,.F.);
#4341=ADVANCED_FACE('',(#602),#427,.T.);
#4342=ADVANCED_FACE('',(#603),#4228,.F.);
#4343=ADVANCED_FACE('',(#604),#428,.T.);
#4344=ADVANCED_FACE('',(#605),#4229,.F.);
#4345=ADVANCED_FACE('',(#606),#4230,.F.);
#4346=ADVANCED_FACE('',(#607),#4231,.F.);
#4347=ADVANCED_FACE('',(#608),#4232,.F.);
#4348=ADVANCED_FACE('',(#609),#4233,.F.);
#4349=ADVANCED_FACE('',(#610),#429,.T.);
#4350=ADVANCED_FACE('',(#611),#430,.T.);
#4351=ADVANCED_FACE('',(#612),#431,.T.);
#4352=ADVANCED_FACE('',(#613),#432,.T.);
#4353=ADVANCED_FACE('',(#614,#294,#295,#296,#297),#433,.T.);
#4354=ADVANCED_FACE('',(#615,#298,#299,#300,#301),#434,.F.);
#4355=ADVANCED_FACE('',(#616),#435,.T.);
#4356=ADVANCED_FACE('',(#617),#4234,.F.);
#4357=ADVANCED_FACE('',(#618),#436,.T.);
#4358=ADVANCED_FACE('',(#619),#4235,.F.);
#4359=ADVANCED_FACE('',(#620),#4236,.F.);
#4360=ADVANCED_FACE('',(#621),#4237,.F.);
#4361=ADVANCED_FACE('',(#622),#4238,.F.);
#4362=ADVANCED_FACE('',(#623),#4239,.F.);
#4363=ADVANCED_FACE('',(#624),#437,.T.);
#4364=ADVANCED_FACE('',(#625),#438,.T.);
#4365=ADVANCED_FACE('',(#626),#439,.T.);
#4366=ADVANCED_FACE('',(#627),#440,.T.);
#4367=ADVANCED_FACE('',(#628,#302,#303,#304,#305),#441,.T.);
#4368=ADVANCED_FACE('',(#629,#306,#307,#308,#309),#442,.F.);
#4369=ADVANCED_FACE('',(#630),#4240,.F.);
#4370=ADVANCED_FACE('',(#631),#4241,.F.);
#4371=ADVANCED_FACE('',(#632),#4242,.F.);
#4372=ADVANCED_FACE('',(#633),#4243,.F.);
#4373=ADVANCED_FACE('',(#634),#4244,.F.);
#4374=ADVANCED_FACE('',(#635),#4245,.F.);
#4375=ADVANCED_FACE('',(#636),#4246,.F.);
#4376=ADVANCED_FACE('',(#637),#4247,.F.);
#4377=ADVANCED_FACE('',(#638),#4248,.F.);
#4378=ADVANCED_FACE('',(#639),#4249,.F.);
#4379=ADVANCED_FACE('',(#640),#4250,.F.);
#4380=ADVANCED_FACE('',(#641),#4251,.F.);
#4381=ADVANCED_FACE('',(#642),#443,.T.);
#4382=ADVANCED_FACE('',(#643),#444,.T.);
#4383=ADVANCED_FACE('',(#644),#445,.T.);
#4384=ADVANCED_FACE('',(#645),#446,.T.);
#4385=ADVANCED_FACE('',(#646,#310,#311,#312,#313,#314,#315,#316,#317,#318,
#319,#320,#321),#447,.T.);
#4386=ADVANCED_FACE('',(#647,#322,#323,#324,#325,#326,#327,#328,#329,#330,
#331,#332,#333),#448,.F.);
#4387=ADVANCED_FACE('',(#648),#4252,.F.);
#4388=ADVANCED_FACE('',(#649),#4253,.F.);
#4389=ADVANCED_FACE('',(#650),#4254,.F.);
#4390=ADVANCED_FACE('',(#651),#4255,.F.);
#4391=ADVANCED_FACE('',(#652),#4256,.F.);
#4392=ADVANCED_FACE('',(#653),#4257,.F.);
#4393=ADVANCED_FACE('',(#654),#4258,.F.);
#4394=ADVANCED_FACE('',(#655),#4259,.F.);
#4395=ADVANCED_FACE('',(#656),#449,.F.);
#4396=ADVANCED_FACE('',(#657),#450,.F.);
#4397=ADVANCED_FACE('',(#658),#451,.F.);
#4398=ADVANCED_FACE('',(#659),#452,.F.);
#4399=ADVANCED_FACE('',(#660),#453,.T.);
#4400=ADVANCED_FACE('',(#661),#454,.T.);
#4401=ADVANCED_FACE('',(#662),#455,.T.);
#4402=ADVANCED_FACE('',(#663),#456,.T.);
#4403=ADVANCED_FACE('',(#664,#334,#335,#336,#337,#338,#339,#340,#341,#342),
#457,.T.);
#4404=ADVANCED_FACE('',(#665,#343,#344,#345,#346,#347,#348,#349,#350,#351),
#458,.F.);
#4405=ADVANCED_FACE('',(#666),#4260,.F.);
#4406=ADVANCED_FACE('',(#667),#459,.F.);
#4407=ADVANCED_FACE('',(#668),#4261,.F.);
#4408=ADVANCED_FACE('',(#669),#460,.F.);
#4409=ADVANCED_FACE('',(#670),#4262,.F.);
#4410=ADVANCED_FACE('',(#671),#461,.F.);
#4411=ADVANCED_FACE('',(#672),#4263,.F.);
#4412=ADVANCED_FACE('',(#673),#462,.F.);
#4413=ADVANCED_FACE('',(#674),#4264,.F.);
#4414=ADVANCED_FACE('',(#675),#463,.F.);
#4415=ADVANCED_FACE('',(#676),#4265,.F.);
#4416=ADVANCED_FACE('',(#677),#464,.F.);
#4417=ADVANCED_FACE('',(#678),#4266,.F.);
#4418=ADVANCED_FACE('',(#679),#465,.F.);
#4419=ADVANCED_FACE('',(#680),#4267,.F.);
#4420=ADVANCED_FACE('',(#681),#466,.F.);
#4421=ADVANCED_FACE('',(#682),#4268,.F.);
#4422=ADVANCED_FACE('',(#683),#467,.F.);
#4423=ADVANCED_FACE('',(#684),#4269,.F.);
#4424=ADVANCED_FACE('',(#685),#468,.F.);
#4425=ADVANCED_FACE('',(#686),#4270,.F.);
#4426=ADVANCED_FACE('',(#687,#352),#469,.T.);
#4427=ADVANCED_FACE('',(#688),#4271,.F.);
#4428=ADVANCED_FACE('',(#689,#353),#470,.F.);
#4429=ADVANCED_FACE('',(#690),#4272,.F.);
#4430=ADVANCED_FACE('',(#691),#4273,.F.);
#4431=ADVANCED_FACE('',(#692,#354),#471,.T.);
#4432=ADVANCED_FACE('',(#693),#4274,.F.);
#4433=ADVANCED_FACE('',(#694),#4275,.F.);
#4434=ADVANCED_FACE('',(#695,#355),#472,.T.);
#4435=ADVANCED_FACE('',(#696),#4276,.F.);
#4436=ADVANCED_FACE('',(#697),#4277,.F.);
#4437=ADVANCED_FACE('',(#698,#356),#473,.T.);
#4438=ADVANCED_FACE('',(#699),#4278,.F.);
#4439=ADVANCED_FACE('',(#700),#4279,.F.);
#4440=ADVANCED_FACE('',(#701,#357),#474,.T.);
#4441=ADVANCED_FACE('',(#702),#475,.F.);
#4442=ADVANCED_FACE('',(#703),#476,.F.);
#4443=ADVANCED_FACE('',(#704),#477,.F.);
#4444=ADVANCED_FACE('',(#705),#478,.F.);
#4445=ADVANCED_FACE('',(#706),#479,.F.);
#4446=ADVANCED_FACE('',(#707),#480,.F.);
#4447=ADVANCED_FACE('',(#708,#358),#4280,.F.);
#4448=ADVANCED_FACE('',(#709),#481,.T.);
#4449=ADVANCED_FACE('',(#710,#359),#482,.T.);
#4450=ADVANCED_FACE('',(#711,#360,#361),#483,.T.);
#4451=ADVANCED_FACE('',(#712,#362),#484,.T.);
#4452=ADVANCED_FACE('',(#713,#363,#364,#365,#366),#485,.T.);
#4453=ADVANCED_FACE('',(#714,#367,#368,#369,#370,#371,#372,#373,#374,#375),
#486,.F.);
#4454=ADVANCED_FACE('',(#715),#4281,.F.);
#4455=ADVANCED_FACE('',(#716),#4282,.T.);
#4456=ADVANCED_FACE('',(#717,#376),#487,.T.);
#4457=ADVANCED_FACE('',(#718,#377),#488,.F.);
#4458=ADVANCED_FACE('',(#719),#4283,.F.);
#4459=ADVANCED_FACE('',(#720),#4284,.T.);
#4460=ADVANCED_FACE('',(#721,#378),#489,.T.);
#4461=ADVANCED_FACE('',(#722,#379),#490,.F.);
#4462=ADVANCED_FACE('',(#723),#4285,.F.);
#4463=ADVANCED_FACE('',(#724),#4286,.T.);
#4464=ADVANCED_FACE('',(#725,#380),#491,.T.);
#4465=ADVANCED_FACE('',(#726,#381),#492,.F.);
#4466=ADVANCED_FACE('',(#727),#4287,.F.);
#4467=ADVANCED_FACE('',(#728),#4288,.T.);
#4468=ADVANCED_FACE('',(#729,#382),#493,.T.);
#4469=ADVANCED_FACE('',(#730,#383),#494,.F.);
#4470=ADVANCED_FACE('',(#731,#384),#495,.F.);
#4471=ADVANCED_FACE('',(#732),#496,.T.);
#4472=ADVANCED_FACE('',(#733),#497,.T.);
#4473=ADVANCED_FACE('',(#734),#498,.T.);
#4474=ADVANCED_FACE('',(#735),#499,.T.);
#4475=ADVANCED_FACE('',(#736),#500,.T.);
#4476=ADVANCED_FACE('',(#737),#501,.T.);
#4477=ADVANCED_FACE('',(#738),#502,.T.);
#4478=ADVANCED_FACE('',(#739),#4289,.T.);
#4479=ADVANCED_FACE('',(#740),#503,.F.);
#4480=ADVANCED_FACE('',(#741),#4290,.T.);
#4481=ADVANCED_FACE('',(#742),#504,.T.);
#4482=ADVANCED_FACE('',(#743),#505,.F.);
#4483=ADVANCED_FACE('',(#744),#4291,.T.);
#4484=ADVANCED_FACE('',(#745),#506,.T.);
#4485=ADVANCED_FACE('',(#746),#507,.F.);
#4486=ADVANCED_FACE('',(#747),#4292,.F.);
#4487=ADVANCED_FACE('',(#748),#4293,.F.);
#4488=ADVANCED_FACE('',(#749,#385,#386),#508,.T.);
#4489=ADVANCED_FACE('',(#750),#509,.T.);
#4490=ADVANCED_FACE('',(#751,#387,#388),#510,.T.);
#4491=ADVANCED_FACE('',(#752),#511,.T.);
#4492=ADVANCED_FACE('',(#753),#512,.T.);
#4493=ADVANCED_FACE('',(#754),#513,.F.);
#4494=ADVANCED_FACE('',(#755),#514,.F.);
#4495=ADVANCED_FACE('',(#756),#515,.F.);
#4496=ADVANCED_FACE('',(#757),#516,.F.);
#4497=ADVANCED_FACE('',(#758),#517,.F.);
#4498=ADVANCED_FACE('',(#759),#518,.F.);
#4499=ADVANCED_FACE('',(#760),#519,.F.);
#4500=ADVANCED_FACE('',(#761),#520,.F.);
#4501=ADVANCED_FACE('',(#762),#521,.F.);
#4502=ADVANCED_FACE('',(#763),#522,.F.);
#4503=ADVANCED_FACE('',(#764),#523,.T.);
#4504=ADVANCED_FACE('',(#765),#167,.T.);
#4505=ADVANCED_FACE('',(#766),#4294,.T.);
#4506=ADVANCED_FACE('',(#767),#168,.T.);
#4507=ADVANCED_FACE('',(#768,#389),#524,.T.);
#4508=ADVANCED_FACE('',(#769),#169,.T.);
#4509=ADVANCED_FACE('',(#770),#4295,.T.);
#4510=ADVANCED_FACE('',(#771),#4296,.F.);
#4511=ADVANCED_FACE('',(#772,#390),#525,.T.);
#4512=ADVANCED_FACE('',(#773,#391),#526,.T.);
#4513=ADVANCED_FACE('',(#774,#392),#527,.F.);
#4514=ADVANCED_FACE('',(#775),#528,.T.);
#4515=ADVANCED_FACE('',(#776),#529,.T.);
#4516=ADVANCED_FACE('',(#777),#530,.T.);
#4517=ADVANCED_FACE('',(#778),#531,.T.);
#4518=ADVANCED_FACE('',(#779),#532,.T.);
#4519=ADVANCED_FACE('',(#780),#533,.T.);
#4520=ADVANCED_FACE('',(#781,#393),#534,.T.);
#4521=ADVANCED_FACE('',(#782),#4297,.F.);
#4522=ADVANCED_FACE('',(#783,#394),#535,.T.);
#4523=ADVANCED_FACE('',(#784),#4298,.T.);
#4524=ADVANCED_FACE('',(#785),#4299,.T.);
#4525=ADVANCED_FACE('',(#786,#395),#536,.T.);
#4526=ADVANCED_FACE('',(#787),#4300,.F.);
#4527=ADVANCED_FACE('',(#788,#396),#537,.T.);
#4528=ADVANCED_FACE('',(#789),#4301,.T.);
#4529=ADVANCED_FACE('',(#790,#397),#538,.T.);
#4530=ADVANCED_FACE('',(#791),#4302,.T.);
#4531=ADVANCED_FACE('',(#792,#398),#539,.T.);
#4532=ADVANCED_FACE('',(#793),#4303,.F.);
#4533=ADVANCED_FACE('',(#794,#399),#540,.F.);
#4534=ADVANCED_FACE('',(#795,#400),#541,.T.);
#4535=ADVANCED_FACE('',(#796),#542,.T.);
#4536=ADVANCED_FACE('',(#797),#543,.T.);
#4537=ADVANCED_FACE('',(#798),#544,.T.);
#4538=ADVANCED_FACE('',(#799),#545,.T.);
#4539=ADVANCED_FACE('',(#800),#546,.T.);
#4540=ADVANCED_FACE('',(#801),#547,.T.);
#4541=ADVANCED_FACE('',(#802),#4304,.T.);
#4542=ADVANCED_FACE('',(#803,#401),#548,.T.);
#4543=ADVANCED_FACE('',(#804),#170,.T.);
#4544=ADVANCED_FACE('',(#805),#4305,.T.);
#4545=ADVANCED_FACE('',(#806),#171,.T.);
#4546=ADVANCED_FACE('',(#807,#402),#549,.T.);
#4547=ADVANCED_FACE('',(#808),#4306,.F.);
#4548=ADVANCED_FACE('',(#809),#550,.T.);
#4549=ADVANCED_FACE('',(#810),#172,.T.);
#4550=ADVANCED_FACE('',(#811),#4307,.T.);
#4551=ADVANCED_FACE('',(#812),#173,.T.);
#4552=ADVANCED_FACE('',(#813,#403),#551,.T.);
#4553=ADVANCED_FACE('',(#814),#174,.T.);
#4554=ADVANCED_FACE('',(#815),#4308,.T.);
#4555=ADVANCED_FACE('',(#816),#175,.T.);
#4556=ADVANCED_FACE('',(#817),#552,.T.);
#4557=ADVANCED_FACE('',(#818),#553,.F.);
#4558=ADVANCED_FACE('',(#819),#554,.F.);
#4559=ADVANCED_FACE('',(#820),#555,.F.);
#4560=ADVANCED_FACE('',(#821),#556,.F.);
#4561=ADVANCED_FACE('',(#822),#557,.F.);
#4562=ADVANCED_FACE('',(#823),#558,.F.);
#4563=ADVANCED_FACE('',(#824),#559,.F.);
#4564=ADVANCED_FACE('',(#825),#560,.F.);
#4565=ADVANCED_FACE('',(#826),#561,.F.);
#4566=ADVANCED_FACE('',(#827),#562,.F.);
#4567=ADVANCED_FACE('',(#828),#563,.F.);
#4568=ADVANCED_FACE('',(#829),#564,.F.);
#4569=ADVANCED_FACE('',(#830),#565,.F.);
#4570=ADVANCED_FACE('',(#831),#566,.F.);
#4571=ADVANCED_FACE('',(#832),#567,.F.);
#4572=ADVANCED_FACE('',(#833),#568,.F.);
#4573=ADVANCED_FACE('',(#834),#569,.F.);
#4574=ADVANCED_FACE('',(#835),#570,.T.);
#4575=ADVANCED_FACE('',(#836),#176,.T.);
#4576=ADVANCED_FACE('',(#837),#4309,.T.);
#4577=ADVANCED_FACE('',(#838),#177,.T.);
#4578=ADVANCED_FACE('',(#839,#404),#571,.T.);
#4579=ADVANCED_FACE('',(#840),#178,.T.);
#4580=ADVANCED_FACE('',(#841),#4310,.T.);
#4581=CLOSED_SHELL('',(#4311,#4312,#4313,#4314,#4315,#4316,#4317,#4318,
#4319,#4320,#4321,#4322,#4323,#4324,#4325,#4326,#4327,#4328));
#4582=CLOSED_SHELL('',(#4329,#4330,#4331,#4332,#4333,#4334));
#4583=CLOSED_SHELL('',(#4335,#4336,#4337,#4338,#4339,#4340));
#4584=CLOSED_SHELL('',(#4341,#4342,#4343,#4344,#4345,#4346,#4347,#4348,
#4349,#4350,#4351,#4352,#4353,#4354));
#4585=CLOSED_SHELL('',(#4355,#4356,#4357,#4358,#4359,#4360,#4361,#4362,
#4363,#4364,#4365,#4366,#4367,#4368));
#4586=CLOSED_SHELL('',(#4369,#4370,#4371,#4372,#4373,#4374,#4375,#4376,
#4377,#4378,#4379,#4380,#4381,#4382,#4383,#4384,#4385,#4386));
#4587=CLOSED_SHELL('',(#4387,#4388,#4389,#4390,#4391,#4392,#4393,#4394,
#4395,#4396,#4397,#4398,#4399,#4400,#4401,#4402,#4403,#4404));
#4588=CLOSED_SHELL('',(#4405,#4406,#4407,#4408,#4409,#4410,#4411,#4412,
#4413,#4414,#4415,#4416,#4417,#4418,#4419,#4420,#4421,#4422,#4423,#4424,
#4425,#4426,#4427,#4428,#4429,#4430,#4431,#4432,#4433,#4434,#4435,#4436,
#4437,#4438,#4439,#4440,#4441,#4442,#4443,#4444,#4445,#4446,#4447,#4448,
#4449,#4450,#4451,#4452,#4453));
#4589=CLOSED_SHELL('',(#4454,#4455,#4456,#4457));
#4590=CLOSED_SHELL('',(#4458,#4459,#4460,#4461));
#4591=CLOSED_SHELL('',(#4462,#4463,#4464,#4465));
#4592=CLOSED_SHELL('',(#4466,#4467,#4468,#4469));
#4593=CLOSED_SHELL('',(#4470,#4471,#4472,#4473,#4474,#4475,#4476,#4477,
#4478,#4479));
#4594=CLOSED_SHELL('',(#4480,#4481,#4482));
#4595=CLOSED_SHELL('',(#4483,#4484,#4485));
#4596=CLOSED_SHELL('',(#4486,#4487,#4488,#4489,#4490,#4491,#4492,#4493));
#4597=CLOSED_SHELL('',(#4494,#4495,#4496,#4497,#4498,#4499,#4500,#4501));
#4598=CLOSED_SHELL('',(#4502,#4503,#4504,#4505,#4506,#4507,#4508,#4509));
#4599=CLOSED_SHELL('',(#4510,#4511,#4512,#4513,#4514,#4515,#4516,#4517,
#4518,#4519,#4520,#4521,#4522,#4523,#4524,#4525,#4526));
#4600=CLOSED_SHELL('',(#4527,#4528,#4529,#4530,#4531,#4532));
#4601=CLOSED_SHELL('',(#4533,#4534,#4535,#4536,#4537,#4538,#4539,#4540,
#4541,#4542,#4543,#4544,#4545,#4546,#4547));
#4602=CLOSED_SHELL('',(#4548,#4549,#4550,#4551,#4552,#4553,#4554,#4555,
#4556));
#4603=CLOSED_SHELL('',(#4557,#4558,#4559,#4560,#4561,#4562,#4563,#4564));
#4604=CLOSED_SHELL('',(#4565,#4566,#4567,#4568,#4569,#4570,#4571,#4572));
#4605=CLOSED_SHELL('',(#4573,#4574,#4575,#4576,#4577,#4578,#4579,#4580));
#4606=DERIVED_UNIT_ELEMENT(#4650,1.);
#4607=DERIVED_UNIT_ELEMENT(#8268,-3.);
#4608=DERIVED_UNIT_ELEMENT(#4650,1.);
#4609=DERIVED_UNIT_ELEMENT(#8268,-3.);
#4610=DERIVED_UNIT_ELEMENT(#4650,1.);
#4611=DERIVED_UNIT_ELEMENT(#8268,-3.);
#4612=DERIVED_UNIT_ELEMENT(#4650,1.);
#4613=DERIVED_UNIT_ELEMENT(#8268,-3.);
#4614=DERIVED_UNIT_ELEMENT(#4650,1.);
#4615=DERIVED_UNIT_ELEMENT(#8268,-3.);
#4616=DERIVED_UNIT_ELEMENT(#4650,1.);
#4617=DERIVED_UNIT_ELEMENT(#8268,-3.);
#4618=DERIVED_UNIT_ELEMENT(#4650,1.);
#4619=DERIVED_UNIT_ELEMENT(#8268,-3.);
#4620=DERIVED_UNIT_ELEMENT(#4650,1.);
#4621=DERIVED_UNIT_ELEMENT(#8268,-3.);
#4622=DERIVED_UNIT_ELEMENT(#4650,1.);
#4623=DERIVED_UNIT_ELEMENT(#8268,-3.);
#4624=DERIVED_UNIT_ELEMENT(#4650,1.);
#4625=DERIVED_UNIT_ELEMENT(#8268,-3.);
#4626=DERIVED_UNIT_ELEMENT(#4650,1.);
#4627=DERIVED_UNIT_ELEMENT(#8268,-3.);
#4628=DERIVED_UNIT_ELEMENT(#4650,1.);
#4629=DERIVED_UNIT_ELEMENT(#8268,-3.);
#4630=DERIVED_UNIT_ELEMENT(#4650,1.);
#4631=DERIVED_UNIT_ELEMENT(#8268,-3.);
#4632=DERIVED_UNIT_ELEMENT(#4650,1.);
#4633=DERIVED_UNIT_ELEMENT(#8268,-3.);
#4634=DERIVED_UNIT_ELEMENT(#4650,1.);
#4635=DERIVED_UNIT_ELEMENT(#8268,-3.);
#4636=DERIVED_UNIT_ELEMENT(#4650,1.);
#4637=DERIVED_UNIT_ELEMENT(#8268,-3.);
#4638=DERIVED_UNIT_ELEMENT(#4650,1.);
#4639=DERIVED_UNIT_ELEMENT(#8268,-3.);
#4640=DERIVED_UNIT_ELEMENT(#4650,1.);
#4641=DERIVED_UNIT_ELEMENT(#8268,-3.);
#4642=DERIVED_UNIT_ELEMENT(#4650,1.);
#4643=DERIVED_UNIT_ELEMENT(#8268,-3.);
#4644=DERIVED_UNIT_ELEMENT(#4650,1.);
#4645=DERIVED_UNIT_ELEMENT(#8268,-3.);
#4646=DERIVED_UNIT_ELEMENT(#4650,1.);
#4647=DERIVED_UNIT_ELEMENT(#8268,-3.);
#4648=DERIVED_UNIT_ELEMENT(#4650,1.);
#4649=DERIVED_UNIT_ELEMENT(#8268,-3.);
#4650=(
MASS_UNIT()
NAMED_UNIT(*)
SI_UNIT(.KILO.,.GRAM.)
);
#4651=DERIVED_UNIT((#4606,#4607));
#4652=DERIVED_UNIT((#4608,#4609));
#4653=DERIVED_UNIT((#4610,#4611));
#4654=DERIVED_UNIT((#4612,#4613));
#4655=DERIVED_UNIT((#4614,#4615));
#4656=DERIVED_UNIT((#4616,#4617));
#4657=DERIVED_UNIT((#4618,#4619));
#4658=DERIVED_UNIT((#4620,#4621));
#4659=DERIVED_UNIT((#4622,#4623));
#4660=DERIVED_UNIT((#4624,#4625));
#4661=DERIVED_UNIT((#4626,#4627));
#4662=DERIVED_UNIT((#4628,#4629));
#4663=DERIVED_UNIT((#4630,#4631));
#4664=DERIVED_UNIT((#4632,#4633));
#4665=DERIVED_UNIT((#4634,#4635));
#4666=DERIVED_UNIT((#4636,#4637));
#4667=DERIVED_UNIT((#4638,#4639));
#4668=DERIVED_UNIT((#4640,#4641));
#4669=DERIVED_UNIT((#4642,#4643));
#4670=DERIVED_UNIT((#4644,#4645));
#4671=DERIVED_UNIT((#4646,#4647));
#4672=DERIVED_UNIT((#4648,#4649));
#4673=MEASURE_REPRESENTATION_ITEM('density measure',
POSITIVE_RATIO_MEASURE(7850.),#4651);
#4674=MEASURE_REPRESENTATION_ITEM('density measure',
POSITIVE_RATIO_MEASURE(7850.),#4652);
#4675=MEASURE_REPRESENTATION_ITEM('density measure',
POSITIVE_RATIO_MEASURE(7850.),#4653);
#4676=MEASURE_REPRESENTATION_ITEM('density measure',
POSITIVE_RATIO_MEASURE(7850.),#4654);
#4677=MEASURE_REPRESENTATION_ITEM('density measure',
POSITIVE_RATIO_MEASURE(7850.),#4655);
#4678=MEASURE_REPRESENTATION_ITEM('density measure',
POSITIVE_RATIO_MEASURE(7850.),#4656);
#4679=MEASURE_REPRESENTATION_ITEM('density measure',
POSITIVE_RATIO_MEASURE(7850.),#4657);
#4680=MEASURE_REPRESENTATION_ITEM('density measure',
POSITIVE_RATIO_MEASURE(7850.),#4658);
#4681=MEASURE_REPRESENTATION_ITEM('density measure',
POSITIVE_RATIO_MEASURE(7850.),#4659);
#4682=MEASURE_REPRESENTATION_ITEM('density measure',
POSITIVE_RATIO_MEASURE(7850.),#4660);
#4683=MEASURE_REPRESENTATION_ITEM('density measure',
POSITIVE_RATIO_MEASURE(7850.),#4661);
#4684=MEASURE_REPRESENTATION_ITEM('density measure',
POSITIVE_RATIO_MEASURE(7850.),#4662);
#4685=MEASURE_REPRESENTATION_ITEM('density measure',
POSITIVE_RATIO_MEASURE(7850.),#4663);
#4686=MEASURE_REPRESENTATION_ITEM('density measure',
POSITIVE_RATIO_MEASURE(7850.),#4664);
#4687=MEASURE_REPRESENTATION_ITEM('density measure',
POSITIVE_RATIO_MEASURE(7850.),#4665);
#4688=MEASURE_REPRESENTATION_ITEM('density measure',
POSITIVE_RATIO_MEASURE(7850.),#4666);
#4689=MEASURE_REPRESENTATION_ITEM('density measure',
POSITIVE_RATIO_MEASURE(7850.),#4667);
#4690=MEASURE_REPRESENTATION_ITEM('density measure',
POSITIVE_RATIO_MEASURE(7850.),#4668);
#4691=MEASURE_REPRESENTATION_ITEM('density measure',
POSITIVE_RATIO_MEASURE(7850.),#4669);
#4692=MEASURE_REPRESENTATION_ITEM('density measure',
POSITIVE_RATIO_MEASURE(7850.),#4670);
#4693=MEASURE_REPRESENTATION_ITEM('density measure',
POSITIVE_RATIO_MEASURE(7850.),#4671);
#4694=MEASURE_REPRESENTATION_ITEM('density measure',
POSITIVE_RATIO_MEASURE(7850.),#4672);
#4695=PROPERTY_DEFINITION_REPRESENTATION(#4805,#4739);
#4696=PROPERTY_DEFINITION_REPRESENTATION(#4806,#4740);
#4697=PROPERTY_DEFINITION_REPRESENTATION(#4807,#4741);
#4698=PROPERTY_DEFINITION_REPRESENTATION(#4808,#4742);
#4699=PROPERTY_DEFINITION_REPRESENTATION(#4809,#4743);
#4700=PROPERTY_DEFINITION_REPRESENTATION(#4810,#4744);
#4701=PROPERTY_DEFINITION_REPRESENTATION(#4811,#4745);
#4702=PROPERTY_DEFINITION_REPRESENTATION(#4812,#4746);
#4703=PROPERTY_DEFINITION_REPRESENTATION(#4813,#4747);
#4704=PROPERTY_DEFINITION_REPRESENTATION(#4814,#4748);
#4705=PROPERTY_DEFINITION_REPRESENTATION(#4815,#4749);
#4706=PROPERTY_DEFINITION_REPRESENTATION(#4816,#4750);
#4707=PROPERTY_DEFINITION_REPRESENTATION(#4817,#4751);
#4708=PROPERTY_DEFINITION_REPRESENTATION(#4818,#4752);
#4709=PROPERTY_DEFINITION_REPRESENTATION(#4819,#4753);
#4710=PROPERTY_DEFINITION_REPRESENTATION(#4820,#4754);
#4711=PROPERTY_DEFINITION_REPRESENTATION(#4821,#4755);
#4712=PROPERTY_DEFINITION_REPRESENTATION(#4822,#4756);
#4713=PROPERTY_DEFINITION_REPRESENTATION(#4823,#4757);
#4714=PROPERTY_DEFINITION_REPRESENTATION(#4824,#4758);
#4715=PROPERTY_DEFINITION_REPRESENTATION(#4825,#4759);
#4716=PROPERTY_DEFINITION_REPRESENTATION(#4826,#4760);
#4717=PROPERTY_DEFINITION_REPRESENTATION(#4827,#4761);
#4718=PROPERTY_DEFINITION_REPRESENTATION(#4828,#4762);
#4719=PROPERTY_DEFINITION_REPRESENTATION(#4829,#4763);
#4720=PROPERTY_DEFINITION_REPRESENTATION(#4830,#4764);
#4721=PROPERTY_DEFINITION_REPRESENTATION(#4831,#4765);
#4722=PROPERTY_DEFINITION_REPRESENTATION(#4832,#4766);
#4723=PROPERTY_DEFINITION_REPRESENTATION(#4833,#4767);
#4724=PROPERTY_DEFINITION_REPRESENTATION(#4834,#4768);
#4725=PROPERTY_DEFINITION_REPRESENTATION(#4835,#4769);
#4726=PROPERTY_DEFINITION_REPRESENTATION(#4836,#4770);
#4727=PROPERTY_DEFINITION_REPRESENTATION(#4837,#4771);
#4728=PROPERTY_DEFINITION_REPRESENTATION(#4838,#4772);
#4729=PROPERTY_DEFINITION_REPRESENTATION(#4839,#4773);
#4730=PROPERTY_DEFINITION_REPRESENTATION(#4840,#4774);
#4731=PROPERTY_DEFINITION_REPRESENTATION(#4841,#4775);
#4732=PROPERTY_DEFINITION_REPRESENTATION(#4842,#4776);
#4733=PROPERTY_DEFINITION_REPRESENTATION(#4843,#4777);
#4734=PROPERTY_DEFINITION_REPRESENTATION(#4844,#4778);
#4735=PROPERTY_DEFINITION_REPRESENTATION(#4845,#4779);
#4736=PROPERTY_DEFINITION_REPRESENTATION(#4846,#4780);
#4737=PROPERTY_DEFINITION_REPRESENTATION(#4847,#4781);
#4738=PROPERTY_DEFINITION_REPRESENTATION(#4848,#4782);
#4739=REPRESENTATION('material name',(#4783),#8243);
#4740=REPRESENTATION('density',(#4673),#8243);
#4741=REPRESENTATION('material name',(#4784),#8244);
#4742=REPRESENTATION('density',(#4674),#8244);
#4743=REPRESENTATION('material name',(#4785),#8245);
#4744=REPRESENTATION('density',(#4675),#8245);
#4745=REPRESENTATION('material name',(#4786),#8246);
#4746=REPRESENTATION('density',(#4676),#8246);
#4747=REPRESENTATION('material name',(#4787),#8247);
#4748=REPRESENTATION('density',(#4677),#8247);
#4749=REPRESENTATION('material name',(#4788),#8248);
#4750=REPRESENTATION('density',(#4678),#8248);
#4751=REPRESENTATION('material name',(#4789),#8249);
#4752=REPRESENTATION('density',(#4679),#8249);
#4753=REPRESENTATION('material name',(#4790),#8250);
#4754=REPRESENTATION('density',(#4680),#8250);
#4755=REPRESENTATION('material name',(#4791),#8251);
#4756=REPRESENTATION('density',(#4681),#8251);
#4757=REPRESENTATION('material name',(#4792),#8252);
#4758=REPRESENTATION('density',(#4682),#8252);
#4759=REPRESENTATION('material name',(#4793),#8253);
#4760=REPRESENTATION('density',(#4683),#8253);
#4761=REPRESENTATION('material name',(#4794),#8254);
#4762=REPRESENTATION('density',(#4684),#8254);
#4763=REPRESENTATION('material name',(#4795),#8255);
#4764=REPRESENTATION('density',(#4685),#8255);
#4765=REPRESENTATION('material name',(#4796),#8256);
#4766=REPRESENTATION('density',(#4686),#8256);
#4767=REPRESENTATION('material name',(#4797),#8257);
#4768=REPRESENTATION('density',(#4687),#8257);
#4769=REPRESENTATION('material name',(#4798),#8258);
#4770=REPRESENTATION('density',(#4688),#8258);
#4771=REPRESENTATION('material name',(#4799),#8259);
#4772=REPRESENTATION('density',(#4689),#8259);
#4773=REPRESENTATION('material name',(#4800),#8261);
#4774=REPRESENTATION('density',(#4690),#8261);
#4775=REPRESENTATION('material name',(#4801),#8262);
#4776=REPRESENTATION('density',(#4691),#8262);
#4777=REPRESENTATION('material name',(#4802),#8263);
#4778=REPRESENTATION('density',(#4692),#8263);
#4779=REPRESENTATION('material name',(#4803),#8264);
#4780=REPRESENTATION('density',(#4693),#8264);
#4781=REPRESENTATION('material name',(#4804),#8265);
#4782=REPRESENTATION('density',(#4694),#8265);
#4783=DESCRIPTIVE_REPRESENTATION_ITEM('Steel','Steel');
#4784=DESCRIPTIVE_REPRESENTATION_ITEM('Steel','Steel');
#4785=DESCRIPTIVE_REPRESENTATION_ITEM('Steel','Steel');
#4786=DESCRIPTIVE_REPRESENTATION_ITEM('Steel','Steel');
#4787=DESCRIPTIVE_REPRESENTATION_ITEM('Steel','Steel');
#4788=DESCRIPTIVE_REPRESENTATION_ITEM('Steel','Steel');
#4789=DESCRIPTIVE_REPRESENTATION_ITEM('Steel','Steel');
#4790=DESCRIPTIVE_REPRESENTATION_ITEM('Steel','Steel');
#4791=DESCRIPTIVE_REPRESENTATION_ITEM('Steel','Steel');
#4792=DESCRIPTIVE_REPRESENTATION_ITEM('Steel','Steel');
#4793=DESCRIPTIVE_REPRESENTATION_ITEM('Steel','Steel');
#4794=DESCRIPTIVE_REPRESENTATION_ITEM('Steel','Steel');
#4795=DESCRIPTIVE_REPRESENTATION_ITEM('Steel','Steel');
#4796=DESCRIPTIVE_REPRESENTATION_ITEM('Steel','Steel');
#4797=DESCRIPTIVE_REPRESENTATION_ITEM('Steel','Steel');
#4798=DESCRIPTIVE_REPRESENTATION_ITEM('Steel','Steel');
#4799=DESCRIPTIVE_REPRESENTATION_ITEM('Steel','Steel');
#4800=DESCRIPTIVE_REPRESENTATION_ITEM('Steel','Steel');
#4801=DESCRIPTIVE_REPRESENTATION_ITEM('Steel','Steel');
#4802=DESCRIPTIVE_REPRESENTATION_ITEM('Steel','Steel');
#4803=DESCRIPTIVE_REPRESENTATION_ITEM('Steel','Steel');
#4804=DESCRIPTIVE_REPRESENTATION_ITEM('Steel','Steel');
#4805=PROPERTY_DEFINITION('material property','material name',#8384);
#4806=PROPERTY_DEFINITION('material property','density of part',#8384);
#4807=PROPERTY_DEFINITION('material property','material name',#8385);
#4808=PROPERTY_DEFINITION('material property','density of part',#8385);
#4809=PROPERTY_DEFINITION('material property','material name',#8386);
#4810=PROPERTY_DEFINITION('material property','density of part',#8386);
#4811=PROPERTY_DEFINITION('material property','material name',#8387);
#4812=PROPERTY_DEFINITION('material property','density of part',#8387);
#4813=PROPERTY_DEFINITION('material property','material name',#8388);
#4814=PROPERTY_DEFINITION('material property','density of part',#8388);
#4815=PROPERTY_DEFINITION('material property','material name',#8389);
#4816=PROPERTY_DEFINITION('material property','density of part',#8389);
#4817=PROPERTY_DEFINITION('material property','material name',#8390);
#4818=PROPERTY_DEFINITION('material property','density of part',#8390);
#4819=PROPERTY_DEFINITION('material property','material name',#8391);
#4820=PROPERTY_DEFINITION('material property','density of part',#8391);
#4821=PROPERTY_DEFINITION('material property','material name',#8392);
#4822=PROPERTY_DEFINITION('material property','density of part',#8392);
#4823=PROPERTY_DEFINITION('material property','material name',#8393);
#4824=PROPERTY_DEFINITION('material property','density of part',#8393);
#4825=PROPERTY_DEFINITION('material property','material name',#8394);
#4826=PROPERTY_DEFINITION('material property','density of part',#8394);
#4827=PROPERTY_DEFINITION('material property','material name',#8395);
#4828=PROPERTY_DEFINITION('material property','density of part',#8395);
#4829=PROPERTY_DEFINITION('material property','material name',#8396);
#4830=PROPERTY_DEFINITION('material property','density of part',#8396);
#4831=PROPERTY_DEFINITION('material property','material name',#8397);
#4832=PROPERTY_DEFINITION('material property','density of part',#8397);
#4833=PROPERTY_DEFINITION('material property','material name',#8398);
#4834=PROPERTY_DEFINITION('material property','density of part',#8398);
#4835=PROPERTY_DEFINITION('material property','material name',#8399);
#4836=PROPERTY_DEFINITION('material property','density of part',#8399);
#4837=PROPERTY_DEFINITION('material property','material name',#8400);
#4838=PROPERTY_DEFINITION('material property','density of part',#8400);
#4839=PROPERTY_DEFINITION('material property','material name',#8402);
#4840=PROPERTY_DEFINITION('material property','density of part',#8402);
#4841=PROPERTY_DEFINITION('material property','material name',#8403);
#4842=PROPERTY_DEFINITION('material property','density of part',#8403);
#4843=PROPERTY_DEFINITION('material property','material name',#8404);
#4844=PROPERTY_DEFINITION('material property','density of part',#8404);
#4845=PROPERTY_DEFINITION('material property','material name',#8405);
#4846=PROPERTY_DEFINITION('material property','density of part',#8405);
#4847=PROPERTY_DEFINITION('material property','material name',#8406);
#4848=PROPERTY_DEFINITION('material property','density of part',#8406);
#4849=AXIS2_PLACEMENT_3D('',#6803,#5382,#5383);
#4850=AXIS2_PLACEMENT_3D('',#6804,#5384,#5385);
#4851=AXIS2_PLACEMENT_3D('',#6805,#5386,#5387);
#4852=AXIS2_PLACEMENT_3D('',#6807,#5388,#5389);
#4853=AXIS2_PLACEMENT_3D('',#6810,#5391,#5392);
#4854=AXIS2_PLACEMENT_3D('',#6811,#5393,#5394);
#4855=AXIS2_PLACEMENT_3D('',#6812,#5395,#5396);
#4856=AXIS2_PLACEMENT_3D('',#6814,#5397,#5398);
#4857=AXIS2_PLACEMENT_3D('',#6817,#5400,#5401);
#4858=AXIS2_PLACEMENT_3D('',#6818,#5402,#5403);
#4859=AXIS2_PLACEMENT_3D('',#6819,#5404,#5405);
#4860=AXIS2_PLACEMENT_3D('',#6821,#5406,#5407);
#4861=AXIS2_PLACEMENT_3D('',#6824,#5409,#5410);
#4862=AXIS2_PLACEMENT_3D('',#6825,#5411,#5412);
#4863=AXIS2_PLACEMENT_3D('',#6826,#5413,#5414);
#4864=AXIS2_PLACEMENT_3D('',#6828,#5415,#5416);
#4865=AXIS2_PLACEMENT_3D('',#6831,#5418,#5419);
#4866=AXIS2_PLACEMENT_3D('',#6832,#5420,#5421);
#4867=AXIS2_PLACEMENT_3D('',#6833,#5422,#5423);
#4868=AXIS2_PLACEMENT_3D('',#6835,#5424,#5425);
#4869=AXIS2_PLACEMENT_3D('',#6838,#5427,#5428);
#4870=AXIS2_PLACEMENT_3D('',#6839,#5429,#5430);
#4871=AXIS2_PLACEMENT_3D('',#6841,#5431,#5432);
#4872=AXIS2_PLACEMENT_3D('',#6844,#5434,#5435);
#4873=AXIS2_PLACEMENT_3D('',#6845,#5436,#5437);
#4874=AXIS2_PLACEMENT_3D('',#6847,#5438,#5439);
#4875=AXIS2_PLACEMENT_3D('',#6850,#5441,#5442);
#4876=AXIS2_PLACEMENT_3D('',#6851,#5443,#5444);
#4877=AXIS2_PLACEMENT_3D('',#6853,#5445,#5446);
#4878=AXIS2_PLACEMENT_3D('',#6856,#5448,#5449);
#4879=AXIS2_PLACEMENT_3D('',#6857,#5450,#5451);
#4880=AXIS2_PLACEMENT_3D('',#6866,#5456,#5457);
#4881=AXIS2_PLACEMENT_3D('',#6872,#5461,#5462);
#4882=AXIS2_PLACEMENT_3D('',#6878,#5466,#5467);
#4883=AXIS2_PLACEMENT_3D('',#6881,#5470,#5471);
#4884=AXIS2_PLACEMENT_3D('',#6882,#5472,#5473);
#4885=AXIS2_PLACEMENT_3D('',#6883,#5474,#5475);
#4886=AXIS2_PLACEMENT_3D('',#6884,#5476,#5477);
#4887=AXIS2_PLACEMENT_3D('',#6893,#5482,#5483);
#4888=AXIS2_PLACEMENT_3D('',#6899,#5487,#5488);
#4889=AXIS2_PLACEMENT_3D('',#6905,#5492,#5493);
#4890=AXIS2_PLACEMENT_3D('',#6908,#5496,#5497);
#4891=AXIS2_PLACEMENT_3D('',#6909,#5498,#5499);
#4892=AXIS2_PLACEMENT_3D('',#6910,#5500,#5501);
#4893=AXIS2_PLACEMENT_3D('',#6911,#5502,#5503);
#4894=AXIS2_PLACEMENT_3D('',#6920,#5508,#5509);
#4895=AXIS2_PLACEMENT_3D('',#6926,#5513,#5514);
#4896=AXIS2_PLACEMENT_3D('',#6932,#5518,#5519);
#4897=AXIS2_PLACEMENT_3D('',#6935,#5522,#5523);
#4898=AXIS2_PLACEMENT_3D('',#6936,#5524,#5525);
#4899=AXIS2_PLACEMENT_3D('',#6937,#5526,#5527);
#4900=AXIS2_PLACEMENT_3D('',#6938,#5528,#5529);
#4901=AXIS2_PLACEMENT_3D('',#6941,#5530,#5531);
#4902=AXIS2_PLACEMENT_3D('',#6942,#5532,#5533);
#4903=AXIS2_PLACEMENT_3D('',#6943,#5534,#5535);
#4904=AXIS2_PLACEMENT_3D('',#6947,#5537,#5538);
#4905=AXIS2_PLACEMENT_3D('',#6949,#5540,#5541);
#4906=AXIS2_PLACEMENT_3D('',#6952,#5542,#5543);
#4907=AXIS2_PLACEMENT_3D('',#6953,#5544,#5545);
#4908=AXIS2_PLACEMENT_3D('',#6954,#5546,#5547);
#4909=AXIS2_PLACEMENT_3D('',#6958,#5549,#5550);
#4910=AXIS2_PLACEMENT_3D('',#6960,#5552,#5553);
#4911=AXIS2_PLACEMENT_3D('',#6962,#5554,#5555);
#4912=AXIS2_PLACEMENT_3D('',#6965,#5557,#5558);
#4913=AXIS2_PLACEMENT_3D('',#6966,#5559,#5560);
#4914=AXIS2_PLACEMENT_3D('',#6967,#5561,#5562);
#4915=AXIS2_PLACEMENT_3D('',#6969,#5563,#5564);
#4916=AXIS2_PLACEMENT_3D('',#6972,#5566,#5567);
#4917=AXIS2_PLACEMENT_3D('',#6973,#5568,#5569);
#4918=AXIS2_PLACEMENT_3D('',#6974,#5570,#5571);
#4919=AXIS2_PLACEMENT_3D('',#6976,#5572,#5573);
#4920=AXIS2_PLACEMENT_3D('',#6979,#5575,#5576);
#4921=AXIS2_PLACEMENT_3D('',#6980,#5577,#5578);
#4922=AXIS2_PLACEMENT_3D('',#6982,#5579,#5580);
#4923=AXIS2_PLACEMENT_3D('',#6985,#5582,#5583);
#4924=AXIS2_PLACEMENT_3D('',#6986,#5584,#5585);
#4925=AXIS2_PLACEMENT_3D('',#6995,#5590,#5591);
#4926=AXIS2_PLACEMENT_3D('',#7001,#5595,#5596);
#4927=AXIS2_PLACEMENT_3D('',#7007,#5600,#5601);
#4928=AXIS2_PLACEMENT_3D('',#7010,#5604,#5605);
#4929=AXIS2_PLACEMENT_3D('',#7011,#5606,#5607);
#4930=AXIS2_PLACEMENT_3D('',#7012,#5608,#5609);
#4931=AXIS2_PLACEMENT_3D('',#7013,#5610,#5611);
#4932=AXIS2_PLACEMENT_3D('',#7016,#5612,#5613);
#4933=AXIS2_PLACEMENT_3D('',#7017,#5614,#5615);
#4934=AXIS2_PLACEMENT_3D('',#7018,#5616,#5617);
#4935=AXIS2_PLACEMENT_3D('',#7022,#5619,#5620);
#4936=AXIS2_PLACEMENT_3D('',#7024,#5622,#5623);
#4937=AXIS2_PLACEMENT_3D('',#7027,#5624,#5625);
#4938=AXIS2_PLACEMENT_3D('',#7028,#5626,#5627);
#4939=AXIS2_PLACEMENT_3D('',#7029,#5628,#5629);
#4940=AXIS2_PLACEMENT_3D('',#7033,#5631,#5632);
#4941=AXIS2_PLACEMENT_3D('',#7035,#5634,#5635);
#4942=AXIS2_PLACEMENT_3D('',#7037,#5636,#5637);
#4943=AXIS2_PLACEMENT_3D('',#7040,#5639,#5640);
#4944=AXIS2_PLACEMENT_3D('',#7041,#5641,#5642);
#4945=AXIS2_PLACEMENT_3D('',#7042,#5643,#5644);
#4946=AXIS2_PLACEMENT_3D('',#7044,#5645,#5646);
#4947=AXIS2_PLACEMENT_3D('',#7047,#5648,#5649);
#4948=AXIS2_PLACEMENT_3D('',#7048,#5650,#5651);
#4949=AXIS2_PLACEMENT_3D('',#7049,#5652,#5653);
#4950=AXIS2_PLACEMENT_3D('',#7051,#5654,#5655);
#4951=AXIS2_PLACEMENT_3D('',#7054,#5657,#5658);
#4952=AXIS2_PLACEMENT_3D('',#7055,#5659,#5660);
#4953=AXIS2_PLACEMENT_3D('',#7057,#5661,#5662);
#4954=AXIS2_PLACEMENT_3D('',#7060,#5664,#5665);
#4955=AXIS2_PLACEMENT_3D('',#7061,#5666,#5667);
#4956=AXIS2_PLACEMENT_3D('',#7070,#5672,#5673);
#4957=AXIS2_PLACEMENT_3D('',#7076,#5677,#5678);
#4958=AXIS2_PLACEMENT_3D('',#7082,#5682,#5683);
#4959=AXIS2_PLACEMENT_3D('',#7085,#5686,#5687);
#4960=AXIS2_PLACEMENT_3D('',#7086,#5688,#5689);
#4961=AXIS2_PLACEMENT_3D('',#7087,#5690,#5691);
#4962=AXIS2_PLACEMENT_3D('',#7088,#5692,#5693);
#4963=AXIS2_PLACEMENT_3D('',#7090,#5694,#5695);
#4964=AXIS2_PLACEMENT_3D('',#7093,#5697,#5698);
#4965=AXIS2_PLACEMENT_3D('',#7094,#5699,#5700);
#4966=AXIS2_PLACEMENT_3D('',#7096,#5701,#5702);
#4967=AXIS2_PLACEMENT_3D('',#7099,#5704,#5705);
#4968=AXIS2_PLACEMENT_3D('',#7100,#5706,#5707);
#4969=AXIS2_PLACEMENT_3D('',#7102,#5708,#5709);
#4970=AXIS2_PLACEMENT_3D('',#7105,#5711,#5712);
#4971=AXIS2_PLACEMENT_3D('',#7106,#5713,#5714);
#4972=AXIS2_PLACEMENT_3D('',#7108,#5715,#5716);
#4973=AXIS2_PLACEMENT_3D('',#7111,#5718,#5719);
#4974=AXIS2_PLACEMENT_3D('',#7112,#5720,#5721);
#4975=AXIS2_PLACEMENT_3D('',#7114,#5722,#5723);
#4976=AXIS2_PLACEMENT_3D('',#7117,#5725,#5726);
#4977=AXIS2_PLACEMENT_3D('',#7118,#5727,#5728);
#4978=AXIS2_PLACEMENT_3D('',#7120,#5729,#5730);
#4979=AXIS2_PLACEMENT_3D('',#7123,#5732,#5733);
#4980=AXIS2_PLACEMENT_3D('',#7124,#5734,#5735);
#4981=AXIS2_PLACEMENT_3D('',#7126,#5736,#5737);
#4982=AXIS2_PLACEMENT_3D('',#7129,#5739,#5740);
#4983=AXIS2_PLACEMENT_3D('',#7130,#5741,#5742);
#4984=AXIS2_PLACEMENT_3D('',#7132,#5743,#5744);
#4985=AXIS2_PLACEMENT_3D('',#7135,#5746,#5747);
#4986=AXIS2_PLACEMENT_3D('',#7136,#5748,#5749);
#4987=AXIS2_PLACEMENT_3D('',#7138,#5750,#5751);
#4988=AXIS2_PLACEMENT_3D('',#7141,#5753,#5754);
#4989=AXIS2_PLACEMENT_3D('',#7142,#5755,#5756);
#4990=AXIS2_PLACEMENT_3D('',#7144,#5757,#5758);
#4991=AXIS2_PLACEMENT_3D('',#7147,#5760,#5761);
#4992=AXIS2_PLACEMENT_3D('',#7148,#5762,#5763);
#4993=AXIS2_PLACEMENT_3D('',#7150,#5764,#5765);
#4994=AXIS2_PLACEMENT_3D('',#7153,#5767,#5768);
#4995=AXIS2_PLACEMENT_3D('',#7154,#5769,#5770);
#4996=AXIS2_PLACEMENT_3D('',#7156,#5771,#5772);
#4997=AXIS2_PLACEMENT_3D('',#7159,#5774,#5775);
#4998=AXIS2_PLACEMENT_3D('',#7160,#5776,#5777);
#4999=AXIS2_PLACEMENT_3D('',#7169,#5782,#5783);
#5000=AXIS2_PLACEMENT_3D('',#7175,#5787,#5788);
#5001=AXIS2_PLACEMENT_3D('',#7181,#5792,#5793);
#5002=AXIS2_PLACEMENT_3D('',#7184,#5796,#5797);
#5003=AXIS2_PLACEMENT_3D('',#7185,#5798,#5799);
#5004=AXIS2_PLACEMENT_3D('',#7186,#5800,#5801);
#5005=AXIS2_PLACEMENT_3D('',#7187,#5802,#5803);
#5006=AXIS2_PLACEMENT_3D('',#7189,#5804,#5805);
#5007=AXIS2_PLACEMENT_3D('',#7192,#5807,#5808);
#5008=AXIS2_PLACEMENT_3D('',#7193,#5809,#5810);
#5009=AXIS2_PLACEMENT_3D('',#7195,#5811,#5812);
#5010=AXIS2_PLACEMENT_3D('',#7198,#5814,#5815);
#5011=AXIS2_PLACEMENT_3D('',#7199,#5816,#5817);
#5012=AXIS2_PLACEMENT_3D('',#7201,#5818,#5819);
#5013=AXIS2_PLACEMENT_3D('',#7204,#5821,#5822);
#5014=AXIS2_PLACEMENT_3D('',#7205,#5823,#5824);
#5015=AXIS2_PLACEMENT_3D('',#7207,#5825,#5826);
#5016=AXIS2_PLACEMENT_3D('',#7210,#5828,#5829);
#5017=AXIS2_PLACEMENT_3D('',#7211,#5830,#5831);
#5018=AXIS2_PLACEMENT_3D('',#7213,#5832,#5833);
#5019=AXIS2_PLACEMENT_3D('',#7216,#5835,#5836);
#5020=AXIS2_PLACEMENT_3D('',#7217,#5837,#5838);
#5021=AXIS2_PLACEMENT_3D('',#7219,#5839,#5840);
#5022=AXIS2_PLACEMENT_3D('',#7222,#5842,#5843);
#5023=AXIS2_PLACEMENT_3D('',#7223,#5844,#5845);
#5024=AXIS2_PLACEMENT_3D('',#7225,#5846,#5847);
#5025=AXIS2_PLACEMENT_3D('',#7228,#5849,#5850);
#5026=AXIS2_PLACEMENT_3D('',#7229,#5851,#5852);
#5027=AXIS2_PLACEMENT_3D('',#7231,#5853,#5854);
#5028=AXIS2_PLACEMENT_3D('',#7234,#5856,#5857);
#5029=AXIS2_PLACEMENT_3D('',#7235,#5858,#5859);
#5030=AXIS2_PLACEMENT_3D('',#7244,#5864,#5865);
#5031=AXIS2_PLACEMENT_3D('',#7250,#5869,#5870);
#5032=AXIS2_PLACEMENT_3D('',#7256,#5874,#5875);
#5033=AXIS2_PLACEMENT_3D('',#7259,#5878,#5879);
#5034=AXIS2_PLACEMENT_3D('',#7268,#5884,#5885);
#5035=AXIS2_PLACEMENT_3D('',#7274,#5889,#5890);
#5036=AXIS2_PLACEMENT_3D('',#7280,#5894,#5895);
#5037=AXIS2_PLACEMENT_3D('',#7283,#5898,#5899);
#5038=AXIS2_PLACEMENT_3D('',#7284,#5900,#5901);
#5039=AXIS2_PLACEMENT_3D('',#7285,#5902,#5903);
#5040=AXIS2_PLACEMENT_3D('',#7286,#5904,#5905);
#5041=AXIS2_PLACEMENT_3D('',#7288,#5906,#5907);
#5042=AXIS2_PLACEMENT_3D('',#7291,#5909,#5910);
#5043=AXIS2_PLACEMENT_3D('',#7292,#5911,#5912);
#5044=AXIS2_PLACEMENT_3D('',#7293,#5913,#5914);
#5045=AXIS2_PLACEMENT_3D('',#7295,#5915,#5916);
#5046=AXIS2_PLACEMENT_3D('',#7298,#5918,#5919);
#5047=AXIS2_PLACEMENT_3D('',#7299,#5920,#5921);
#5048=AXIS2_PLACEMENT_3D('',#7300,#5922,#5923);
#5049=AXIS2_PLACEMENT_3D('',#7302,#5924,#5925);
#5050=AXIS2_PLACEMENT_3D('',#7305,#5927,#5928);
#5051=AXIS2_PLACEMENT_3D('',#7306,#5929,#5930);
#5052=AXIS2_PLACEMENT_3D('',#7307,#5931,#5932);
#5053=AXIS2_PLACEMENT_3D('',#7309,#5933,#5934);
#5054=AXIS2_PLACEMENT_3D('',#7312,#5936,#5937);
#5055=AXIS2_PLACEMENT_3D('',#7313,#5938,#5939);
#5056=AXIS2_PLACEMENT_3D('',#7314,#5940,#5941);
#5057=AXIS2_PLACEMENT_3D('',#7316,#5942,#5943);
#5058=AXIS2_PLACEMENT_3D('',#7319,#5945,#5946);
#5059=AXIS2_PLACEMENT_3D('',#7320,#5947,#5948);
#5060=AXIS2_PLACEMENT_3D('',#7321,#5949,#5950);
#5061=AXIS2_PLACEMENT_3D('',#7323,#5951,#5952);
#5062=AXIS2_PLACEMENT_3D('',#7326,#5954,#5955);
#5063=AXIS2_PLACEMENT_3D('',#7327,#5956,#5957);
#5064=AXIS2_PLACEMENT_3D('',#7328,#5958,#5959);
#5065=AXIS2_PLACEMENT_3D('',#7330,#5960,#5961);
#5066=AXIS2_PLACEMENT_3D('',#7333,#5963,#5964);
#5067=AXIS2_PLACEMENT_3D('',#7334,#5965,#5966);
#5068=AXIS2_PLACEMENT_3D('',#7335,#5967,#5968);
#5069=AXIS2_PLACEMENT_3D('',#7337,#5969,#5970);
#5070=AXIS2_PLACEMENT_3D('',#7340,#5972,#5973);
#5071=AXIS2_PLACEMENT_3D('',#7341,#5974,#5975);
#5072=AXIS2_PLACEMENT_3D('',#7342,#5976,#5977);
#5073=AXIS2_PLACEMENT_3D('',#7344,#5978,#5979);
#5074=AXIS2_PLACEMENT_3D('',#7347,#5981,#5982);
#5075=AXIS2_PLACEMENT_3D('',#7348,#5983,#5984);
#5076=AXIS2_PLACEMENT_3D('',#7349,#5985,#5986);
#5077=AXIS2_PLACEMENT_3D('',#7351,#5987,#5988);
#5078=AXIS2_PLACEMENT_3D('',#7354,#5990,#5991);
#5079=AXIS2_PLACEMENT_3D('',#7355,#5992,#5993);
#5080=AXIS2_PLACEMENT_3D('',#7356,#5994,#5995);
#5081=AXIS2_PLACEMENT_3D('',#7358,#5996,#5997);
#5082=AXIS2_PLACEMENT_3D('',#7361,#5999,#6000);
#5083=AXIS2_PLACEMENT_3D('',#7362,#6001,#6002);
#5084=AXIS2_PLACEMENT_3D('',#7364,#6003,#6004);
#5085=AXIS2_PLACEMENT_3D('',#7365,#6005,#6006);
#5086=AXIS2_PLACEMENT_3D('',#7367,#6007,#6008);
#5087=AXIS2_PLACEMENT_3D('',#7370,#6010,#6011);
#5088=AXIS2_PLACEMENT_3D('',#7371,#6012,#6013);
#5089=AXIS2_PLACEMENT_3D('',#7373,#6014,#6015);
#5090=AXIS2_PLACEMENT_3D('',#7374,#6016,#6017);
#5091=AXIS2_PLACEMENT_3D('',#7400,#6019,#6020);
#5092=AXIS2_PLACEMENT_3D('',#7419,#6021,#6022);
#5093=AXIS2_PLACEMENT_3D('',#7421,#6023,#6024);
#5094=AXIS2_PLACEMENT_3D('',#7424,#6026,#6027);
#5095=AXIS2_PLACEMENT_3D('',#7425,#6028,#6029);
#5096=AXIS2_PLACEMENT_3D('',#7426,#6030,#6031);
#5097=AXIS2_PLACEMENT_3D('',#7452,#6033,#6034);
#5098=AXIS2_PLACEMENT_3D('',#7471,#6035,#6036);
#5099=AXIS2_PLACEMENT_3D('',#7473,#6037,#6038);
#5100=AXIS2_PLACEMENT_3D('',#7476,#6040,#6041);
#5101=AXIS2_PLACEMENT_3D('',#7477,#6042,#6043);
#5102=AXIS2_PLACEMENT_3D('',#7478,#6044,#6045);
#5103=AXIS2_PLACEMENT_3D('',#7504,#6047,#6048);
#5104=AXIS2_PLACEMENT_3D('',#7523,#6049,#6050);
#5105=AXIS2_PLACEMENT_3D('',#7525,#6051,#6052);
#5106=AXIS2_PLACEMENT_3D('',#7528,#6054,#6055);
#5107=AXIS2_PLACEMENT_3D('',#7529,#6056,#6057);
#5108=AXIS2_PLACEMENT_3D('',#7530,#6058,#6059);
#5109=AXIS2_PLACEMENT_3D('',#7556,#6061,#6062);
#5110=AXIS2_PLACEMENT_3D('',#7575,#6063,#6064);
#5111=AXIS2_PLACEMENT_3D('',#7577,#6065,#6066);
#5112=AXIS2_PLACEMENT_3D('',#7580,#6068,#6069);
#5113=AXIS2_PLACEMENT_3D('',#7581,#6070,#6071);
#5114=AXIS2_PLACEMENT_3D('',#7582,#6072,#6073);
#5115=AXIS2_PLACEMENT_3D('',#7591,#6078,#6079);
#5116=AXIS2_PLACEMENT_3D('',#7597,#6082,#6083);
#5117=AXIS2_PLACEMENT_3D('',#7601,#6086,#6087);
#5118=AXIS2_PLACEMENT_3D('',#7605,#6090,#6091);
#5119=AXIS2_PLACEMENT_3D('',#7611,#6095,#6096);
#5120=AXIS2_PLACEMENT_3D('',#7615,#6099,#6100);
#5121=AXIS2_PLACEMENT_3D('',#7616,#6101,#6102);
#5122=AXIS2_PLACEMENT_3D('',#7618,#6104,#6105);
#5123=AXIS2_PLACEMENT_3D('',#7624,#6111,#6112);
#5124=AXIS2_PLACEMENT_3D('',#7633,#6117,#6118);
#5125=AXIS2_PLACEMENT_3D('',#7639,#6122,#6123);
#5126=AXIS2_PLACEMENT_3D('',#7645,#6127,#6128);
#5127=AXIS2_PLACEMENT_3D('',#7648,#6131,#6132);
#5128=AXIS2_PLACEMENT_3D('',#7649,#6133,#6134);
#5129=AXIS2_PLACEMENT_3D('',#7650,#6135,#6136);
#5130=AXIS2_PLACEMENT_3D('',#7651,#6137,#6138);
#5131=AXIS2_PLACEMENT_3D('',#7653,#6139,#6140);
#5132=AXIS2_PLACEMENT_3D('',#7656,#6142,#6143);
#5133=AXIS2_PLACEMENT_3D('',#7657,#6144,#6145);
#5134=AXIS2_PLACEMENT_3D('',#7659,#6146,#6147);
#5135=AXIS2_PLACEMENT_3D('',#7662,#6149,#6150);
#5136=AXIS2_PLACEMENT_3D('',#7663,#6151,#6152);
#5137=AXIS2_PLACEMENT_3D('',#7664,#6153,#6154);
#5138=AXIS2_PLACEMENT_3D('',#7665,#6155,#6156);
#5139=AXIS2_PLACEMENT_3D('',#7666,#6157,#6158);
#5140=AXIS2_PLACEMENT_3D('',#7668,#6159,#6160);
#5141=AXIS2_PLACEMENT_3D('',#7671,#6162,#6163);
#5142=AXIS2_PLACEMENT_3D('',#7672,#6164,#6165);
#5143=AXIS2_PLACEMENT_3D('',#7674,#6166,#6167);
#5144=AXIS2_PLACEMENT_3D('',#7677,#6169,#6170);
#5145=AXIS2_PLACEMENT_3D('',#7678,#6171,#6172);
#5146=AXIS2_PLACEMENT_3D('',#7679,#6173,#6174);
#5147=AXIS2_PLACEMENT_3D('',#7680,#6175,#6176);
#5148=AXIS2_PLACEMENT_3D('',#7681,#6177,#6178);
#5149=AXIS2_PLACEMENT_3D('',#7683,#6179,#6180);
#5150=AXIS2_PLACEMENT_3D('',#7686,#6182,#6183);
#5151=AXIS2_PLACEMENT_3D('',#7687,#6184,#6185);
#5152=AXIS2_PLACEMENT_3D('',#7689,#6186,#6187);
#5153=AXIS2_PLACEMENT_3D('',#7692,#6189,#6190);
#5154=AXIS2_PLACEMENT_3D('',#7693,#6191,#6192);
#5155=AXIS2_PLACEMENT_3D('',#7694,#6193,#6194);
#5156=AXIS2_PLACEMENT_3D('',#7695,#6195,#6196);
#5157=AXIS2_PLACEMENT_3D('',#7696,#6197,#6198);
#5158=AXIS2_PLACEMENT_3D('',#7698,#6199,#6200);
#5159=AXIS2_PLACEMENT_3D('',#7701,#6202,#6203);
#5160=AXIS2_PLACEMENT_3D('',#7702,#6204,#6205);
#5161=AXIS2_PLACEMENT_3D('',#7704,#6206,#6207);
#5162=AXIS2_PLACEMENT_3D('',#7707,#6209,#6210);
#5163=AXIS2_PLACEMENT_3D('',#7708,#6211,#6212);
#5164=AXIS2_PLACEMENT_3D('',#7709,#6213,#6214);
#5165=AXIS2_PLACEMENT_3D('',#7710,#6215,#6216);
#5166=AXIS2_PLACEMENT_3D('',#7711,#6217,#6218);
#5167=AXIS2_PLACEMENT_3D('',#7725,#6225,#6226);
#5168=AXIS2_PLACEMENT_3D('',#7726,#6227,#6228);
#5169=AXIS2_PLACEMENT_3D('',#7732,#6232,#6233);
#5170=AXIS2_PLACEMENT_3D('',#7736,#6236,#6237);
#5171=AXIS2_PLACEMENT_3D('',#7740,#6240,#6241);
#5172=AXIS2_PLACEMENT_3D('',#7744,#6244,#6245);
#5173=AXIS2_PLACEMENT_3D('',#7748,#6248,#6249);
#5174=AXIS2_PLACEMENT_3D('',#7750,#6251,#6252);
#5175=AXIS2_PLACEMENT_3D('',#7751,#6253,#6254);
#5176=AXIS2_PLACEMENT_3D('',#7754,#6256,#6257);
#5177=AXIS2_PLACEMENT_3D('',#7755,#6258,#6259);
#5178=AXIS2_PLACEMENT_3D('',#7756,#6260,#6261);
#5179=AXIS2_PLACEMENT_3D('',#7757,#6262,#6263);
#5180=AXIS2_PLACEMENT_3D('',#7759,#6264,#6265);
#5181=AXIS2_PLACEMENT_3D('',#7762,#6267,#6268);
#5182=AXIS2_PLACEMENT_3D('',#7763,#6269,#6270);
#5183=AXIS2_PLACEMENT_3D('',#7764,#6271,#6272);
#5184=AXIS2_PLACEMENT_3D('',#7765,#6273,#6274);
#5185=AXIS2_PLACEMENT_3D('',#7766,#6275,#6276);
#5186=AXIS2_PLACEMENT_3D('',#7768,#6277,#6278);
#5187=AXIS2_PLACEMENT_3D('',#7771,#6280,#6281);
#5188=AXIS2_PLACEMENT_3D('',#7772,#6282,#6283);
#5189=AXIS2_PLACEMENT_3D('',#7773,#6284,#6285);
#5190=AXIS2_PLACEMENT_3D('',#7774,#6286,#6287);
#5191=AXIS2_PLACEMENT_3D('',#7775,#6288,#6289);
#5192=AXIS2_PLACEMENT_3D('',#7777,#6290,#6291);
#5193=AXIS2_PLACEMENT_3D('',#7780,#6293,#6294);
#5194=AXIS2_PLACEMENT_3D('',#7781,#6295,#6296);
#5195=AXIS2_PLACEMENT_3D('',#7783,#6297,#6298);
#5196=AXIS2_PLACEMENT_3D('',#7786,#6300,#6301);
#5197=AXIS2_PLACEMENT_3D('',#7787,#6302,#6303);
#5198=AXIS2_PLACEMENT_3D('',#7796,#6308,#6309);
#5199=AXIS2_PLACEMENT_3D('',#7802,#6313,#6314);
#5200=AXIS2_PLACEMENT_3D('',#7808,#6318,#6319);
#5201=AXIS2_PLACEMENT_3D('',#7811,#6322,#6323);
#5202=AXIS2_PLACEMENT_3D('',#7812,#6324,#6325);
#5203=AXIS2_PLACEMENT_3D('',#7813,#6326,#6327);
#5204=AXIS2_PLACEMENT_3D('',#7814,#6328,#6329);
#5205=AXIS2_PLACEMENT_3D('',#7823,#6334,#6335);
#5206=AXIS2_PLACEMENT_3D('',#7829,#6339,#6340);
#5207=AXIS2_PLACEMENT_3D('',#7835,#6344,#6345);
#5208=AXIS2_PLACEMENT_3D('',#7841,#6349,#6350);
#5209=AXIS2_PLACEMENT_3D('',#7847,#6354,#6355);
#5210=AXIS2_PLACEMENT_3D('',#7850,#6358,#6359);
#5211=AXIS2_PLACEMENT_3D('',#7851,#6360,#6361);
#5212=AXIS2_PLACEMENT_3D('',#7852,#6362,#6363);
#5213=AXIS2_PLACEMENT_3D('',#7854,#6364,#6365);
#5214=AXIS2_PLACEMENT_3D('',#7855,#6366,#6367);
#5215=AXIS2_PLACEMENT_3D('',#7857,#6368,#6369);
#5216=AXIS2_PLACEMENT_3D('',#7858,#6370,#6371);
#5217=AXIS2_PLACEMENT_3D('',#7860,#6372,#6373);
#5218=AXIS2_PLACEMENT_3D('',#7862,#6375,#6376);
#5219=AXIS2_PLACEMENT_3D('',#7864,#6377,#6378);
#5220=AXIS2_PLACEMENT_3D('',#7866,#6380,#6381);
#5221=AXIS2_PLACEMENT_3D('',#7868,#6382,#6383);
#5222=AXIS2_PLACEMENT_3D('',#7870,#6385,#6386);
#5223=AXIS2_PLACEMENT_3D('',#7872,#6387,#6388);
#5224=AXIS2_PLACEMENT_3D('',#7873,#6389,#6390);
#5225=AXIS2_PLACEMENT_3D('',#7875,#6391,#6392);
#5226=AXIS2_PLACEMENT_3D('',#7877,#6394,#6395);
#5227=AXIS2_PLACEMENT_3D('',#7879,#6397,#6398);
#5228=AXIS2_PLACEMENT_3D('',#7880,#6399,#6400);
#5229=AXIS2_PLACEMENT_3D('',#7881,#6401,#6402);
#5230=AXIS2_PLACEMENT_3D('',#7883,#6403,#6404);
#5231=AXIS2_PLACEMENT_3D('',#7886,#6406,#6407);
#5232=AXIS2_PLACEMENT_3D('',#7887,#6408,#6409);
#5233=AXIS2_PLACEMENT_3D('',#7889,#6410,#6411);
#5234=AXIS2_PLACEMENT_3D('',#7890,#6412,#6413);
#5235=AXIS2_PLACEMENT_3D('',#7904,#6420,#6421);
#5236=AXIS2_PLACEMENT_3D('',#7905,#6422,#6423);
#5237=AXIS2_PLACEMENT_3D('',#7919,#6430,#6431);
#5238=AXIS2_PLACEMENT_3D('',#7920,#6432,#6433);
#5239=AXIS2_PLACEMENT_3D('',#7923,#6436,#6437);
#5240=AXIS2_PLACEMENT_3D('',#7925,#6439,#6440);
#5241=AXIS2_PLACEMENT_3D('',#7927,#6442,#6443);
#5242=AXIS2_PLACEMENT_3D('',#7929,#6445,#6446);
#5243=AXIS2_PLACEMENT_3D('',#7931,#6448,#6449);
#5244=AXIS2_PLACEMENT_3D('',#7932,#6450,#6451);
#5245=AXIS2_PLACEMENT_3D('',#7934,#6452,#6453);
#5246=AXIS2_PLACEMENT_3D('',#7935,#6454,#6455);
#5247=AXIS2_PLACEMENT_3D('',#7938,#6457,#6458);
#5248=AXIS2_PLACEMENT_3D('',#7939,#6459,#6460);
#5249=AXIS2_PLACEMENT_3D('',#7941,#6461,#6462);
#5250=AXIS2_PLACEMENT_3D('',#7942,#6463,#6464);
#5251=AXIS2_PLACEMENT_3D('',#7944,#6466,#6467);
#5252=AXIS2_PLACEMENT_3D('',#7946,#6468,#6469);
#5253=AXIS2_PLACEMENT_3D('',#7948,#6471,#6472);
#5254=AXIS2_PLACEMENT_3D('',#7950,#6473,#6474);
#5255=AXIS2_PLACEMENT_3D('',#7951,#6475,#6476);
#5256=AXIS2_PLACEMENT_3D('',#7953,#6478,#6479);
#5257=AXIS2_PLACEMENT_3D('',#7954,#6480,#6481);
#5258=AXIS2_PLACEMENT_3D('',#7956,#6482,#6483);
#5259=AXIS2_PLACEMENT_3D('',#7958,#6484,#6485);
#5260=AXIS2_PLACEMENT_3D('',#7959,#6486,#6487);
#5261=AXIS2_PLACEMENT_3D('',#7961,#6488,#6489);
#5262=AXIS2_PLACEMENT_3D('',#7963,#6491,#6492);
#5263=AXIS2_PLACEMENT_3D('',#7965,#6493,#6494);
#5264=AXIS2_PLACEMENT_3D('',#7966,#6495,#6496);
#5265=AXIS2_PLACEMENT_3D('',#7968,#6497,#6498);
#5266=AXIS2_PLACEMENT_3D('',#7970,#6500,#6501);
#5267=AXIS2_PLACEMENT_3D('',#7972,#6502,#6503);
#5268=AXIS2_PLACEMENT_3D('',#7973,#6504,#6505);
#5269=AXIS2_PLACEMENT_3D('',#7975,#6507,#6508);
#5270=AXIS2_PLACEMENT_3D('',#7976,#6509,#6510);
#5271=AXIS2_PLACEMENT_3D('',#7977,#6511,#6512);
#5272=AXIS2_PLACEMENT_3D('',#7978,#6513,#6514);
#5273=AXIS2_PLACEMENT_3D('',#7992,#6521,#6522);
#5274=AXIS2_PLACEMENT_3D('',#7993,#6523,#6524);
#5275=AXIS2_PLACEMENT_3D('',#8007,#6531,#6532);
#5276=AXIS2_PLACEMENT_3D('',#8008,#6533,#6534);
#5277=AXIS2_PLACEMENT_3D('',#8011,#6537,#6538);
#5278=AXIS2_PLACEMENT_3D('',#8013,#6540,#6541);
#5279=AXIS2_PLACEMENT_3D('',#8015,#6543,#6544);
#5280=AXIS2_PLACEMENT_3D('',#8017,#6546,#6547);
#5281=AXIS2_PLACEMENT_3D('',#8019,#6549,#6550);
#5282=AXIS2_PLACEMENT_3D('',#8020,#6551,#6552);
#5283=AXIS2_PLACEMENT_3D('',#8023,#6554,#6555);
#5284=AXIS2_PLACEMENT_3D('',#8024,#6556,#6557);
#5285=AXIS2_PLACEMENT_3D('',#8026,#6558,#6559);
#5286=AXIS2_PLACEMENT_3D('',#8028,#6560,#6561);
#5287=AXIS2_PLACEMENT_3D('',#8029,#6562,#6563);
#5288=AXIS2_PLACEMENT_3D('',#8031,#6565,#6566);
#5289=AXIS2_PLACEMENT_3D('',#8033,#6567,#6568);
#5290=AXIS2_PLACEMENT_3D('',#8035,#6570,#6571);
#5291=AXIS2_PLACEMENT_3D('',#8037,#6572,#6573);
#5292=AXIS2_PLACEMENT_3D('',#8039,#6575,#6576);
#5293=AXIS2_PLACEMENT_3D('',#8041,#6577,#6578);
#5294=AXIS2_PLACEMENT_3D('',#8042,#6579,#6580);
#5295=AXIS2_PLACEMENT_3D('',#8044,#6582,#6583);
#5296=AXIS2_PLACEMENT_3D('',#8045,#6584,#6585);
#5297=AXIS2_PLACEMENT_3D('',#8047,#6586,#6587);
#5298=AXIS2_PLACEMENT_3D('',#8048,#6588,#6589);
#5299=AXIS2_PLACEMENT_3D('',#8050,#6590,#6591);
#5300=AXIS2_PLACEMENT_3D('',#8052,#6593,#6594);
#5301=AXIS2_PLACEMENT_3D('',#8054,#6595,#6596);
#5302=AXIS2_PLACEMENT_3D('',#8056,#6598,#6599);
#5303=AXIS2_PLACEMENT_3D('',#8058,#6600,#6601);
#5304=AXIS2_PLACEMENT_3D('',#8060,#6603,#6604);
#5305=AXIS2_PLACEMENT_3D('',#8062,#6605,#6606);
#5306=AXIS2_PLACEMENT_3D('',#8063,#6607,#6608);
#5307=AXIS2_PLACEMENT_3D('',#8065,#6609,#6610);
#5308=AXIS2_PLACEMENT_3D('',#8067,#6612,#6613);
#5309=AXIS2_PLACEMENT_3D('',#8069,#6614,#6615);
#5310=AXIS2_PLACEMENT_3D('',#8071,#6617,#6618);
#5311=AXIS2_PLACEMENT_3D('',#8073,#6619,#6620);
#5312=AXIS2_PLACEMENT_3D('',#8075,#6622,#6623);
#5313=AXIS2_PLACEMENT_3D('',#8076,#6624,#6625);
#5314=AXIS2_PLACEMENT_3D('',#8085,#6630,#6631);
#5315=AXIS2_PLACEMENT_3D('',#8091,#6635,#6636);
#5316=AXIS2_PLACEMENT_3D('',#8097,#6640,#6641);
#5317=AXIS2_PLACEMENT_3D('',#8103,#6645,#6646);
#5318=AXIS2_PLACEMENT_3D('',#8109,#6650,#6651);
#5319=AXIS2_PLACEMENT_3D('',#8112,#6654,#6655);
#5320=AXIS2_PLACEMENT_3D('',#8113,#6656,#6657);
#5321=AXIS2_PLACEMENT_3D('',#8114,#6658,#6659);
#5322=AXIS2_PLACEMENT_3D('',#8115,#6660,#6661);
#5323=AXIS2_PLACEMENT_3D('',#8124,#6666,#6667);
#5324=AXIS2_PLACEMENT_3D('',#8130,#6671,#6672);
#5325=AXIS2_PLACEMENT_3D('',#8136,#6676,#6677);
#5326=AXIS2_PLACEMENT_3D('',#8142,#6681,#6682);
#5327=AXIS2_PLACEMENT_3D('',#8148,#6686,#6687);
#5328=AXIS2_PLACEMENT_3D('',#8151,#6690,#6691);
#5329=AXIS2_PLACEMENT_3D('',#8152,#6692,#6693);
#5330=AXIS2_PLACEMENT_3D('',#8153,#6694,#6695);
#5331=AXIS2_PLACEMENT_3D('',#8155,#6696,#6697);
#5332=AXIS2_PLACEMENT_3D('',#8156,#6698,#6699);
#5333=AXIS2_PLACEMENT_3D('',#8158,#6700,#6701);
#5334=AXIS2_PLACEMENT_3D('',#8159,#6702,#6703);
#5335=AXIS2_PLACEMENT_3D('',#8161,#6704,#6705);
#5336=AXIS2_PLACEMENT_3D('',#8163,#6707,#6708);
#5337=AXIS2_PLACEMENT_3D('',#8165,#6709,#6710);
#5338=AXIS2_PLACEMENT_3D('',#8167,#6712,#6713);
#5339=AXIS2_PLACEMENT_3D('',#8169,#6714,#6715);
#5340=AXIS2_PLACEMENT_3D('',#8171,#6717,#6718);
#5341=AXIS2_PLACEMENT_3D('',#8173,#6719,#6720);
#5342=AXIS2_PLACEMENT_3D('',#8174,#6721,#6722);
#5343=AXIS2_PLACEMENT_3D('',#8176,#6723,#6724);
#5344=AXIS2_PLACEMENT_3D('',#8178,#6726,#6727);
#5345=AXIS2_PLACEMENT_3D('',#8180,#6729,#6730);
#5346=AXIS2_PLACEMENT_3D('',#8181,#6731,#6732);
#5347=AXIS2_PLACEMENT_3D('',#8182,#6733,#6734);
#5348=AXIS2_PLACEMENT_3D('',#8183,#6735,#6736);
#5349=AXIS2_PLACEMENT_3D('',#8184,#6737,#6738);
#5350=AXIS2_PLACEMENT_3D('',#8185,#6739,#6740);
#5351=AXIS2_PLACEMENT_3D('',#8186,#6741,#6742);
#5352=AXIS2_PLACEMENT_3D('',#8187,#6743,#6744);
#5353=AXIS2_PLACEMENT_3D('',#8188,#6745,#6746);
#5354=AXIS2_PLACEMENT_3D('',#8189,#6747,#6748);
#5355=AXIS2_PLACEMENT_3D('',#8190,#6749,#6750);
#5356=AXIS2_PLACEMENT_3D('',#8191,#6751,#6752);
#5357=AXIS2_PLACEMENT_3D('',#8192,#6753,#6754);
#5358=AXIS2_PLACEMENT_3D('',#8193,#6755,#6756);
#5359=AXIS2_PLACEMENT_3D('',#8194,#6757,#6758);
#5360=AXIS2_PLACEMENT_3D('',#8195,#6759,#6760);
#5361=AXIS2_PLACEMENT_3D('',#8196,#6761,#6762);
#5362=AXIS2_PLACEMENT_3D('',#8197,#6763,#6764);
#5363=AXIS2_PLACEMENT_3D('',#8198,#6765,#6766);
#5364=AXIS2_PLACEMENT_3D('',#8199,#6767,#6768);
#5365=AXIS2_PLACEMENT_3D('',#8200,#6769,#6770);
#5366=AXIS2_PLACEMENT_3D('',#8201,#6771,#6772);
#5367=AXIS2_PLACEMENT_3D('',#8202,#6773,#6774);
#5368=AXIS2_PLACEMENT_3D('',#8203,#6775,#6776);
#5369=AXIS2_PLACEMENT_3D('',#8204,#6777,#6778);
#5370=AXIS2_PLACEMENT_3D('',#8205,#6779,#6780);
#5371=AXIS2_PLACEMENT_3D('',#8206,#6781,#6782);
#5372=AXIS2_PLACEMENT_3D('',#8207,#6783,#6784);
#5373=AXIS2_PLACEMENT_3D('',#8208,#6785,#6786);
#5374=AXIS2_PLACEMENT_3D('',#8209,#6787,#6788);
#5375=AXIS2_PLACEMENT_3D('',#8210,#6789,#6790);
#5376=AXIS2_PLACEMENT_3D('',#8211,#6791,#6792);
#5377=AXIS2_PLACEMENT_3D('',#8212,#6793,#6794);
#5378=AXIS2_PLACEMENT_3D('',#8213,#6795,#6796);
#5379=AXIS2_PLACEMENT_3D('',#8214,#6797,#6798);
#5380=AXIS2_PLACEMENT_3D('',#8215,#6799,#6800);
#5381=AXIS2_PLACEMENT_3D('',#8216,#6801,#6802);
#5382=DIRECTION('axis',(0.,0.,1.));
#5383=DIRECTION('refdir',(1.,0.,0.));
#5384=DIRECTION('axis',(0.,0.,1.));
#5385=DIRECTION('refdir',(1.,0.,0.));
#5386=DIRECTION('center_axis',(0.,0.,1.));
#5387=DIRECTION('ref_axis',(1.,0.,0.));
#5388=DIRECTION('center_axis',(0.,0.,1.));
#5389=DIRECTION('ref_axis',(1.,0.,0.));
#5390=DIRECTION('',(0.,0.,1.));
#5391=DIRECTION('center_axis',(0.,0.,-1.));
#5392=DIRECTION('ref_axis',(1.,0.,0.));
#5393=DIRECTION('center_axis',(0.,0.,1.));
#5394=DIRECTION('ref_axis',(1.,0.,0.));
#5395=DIRECTION('center_axis',(0.,0.,1.));
#5396=DIRECTION('ref_axis',(1.,0.,0.));
#5397=DIRECTION('center_axis',(0.,0.,1.));
#5398=DIRECTION('ref_axis',(1.,0.,0.));
#5399=DIRECTION('',(0.,0.,1.));
#5400=DIRECTION('center_axis',(0.,0.,-1.));
#5401=DIRECTION('ref_axis',(1.,0.,0.));
#5402=DIRECTION('center_axis',(0.,0.,1.));
#5403=DIRECTION('ref_axis',(1.,0.,0.));
#5404=DIRECTION('center_axis',(0.,0.,1.));
#5405=DIRECTION('ref_axis',(1.,0.,0.));
#5406=DIRECTION('center_axis',(0.,0.,1.));
#5407=DIRECTION('ref_axis',(1.,0.,0.));
#5408=DIRECTION('',(0.,0.,1.));
#5409=DIRECTION('center_axis',(0.,0.,-1.));
#5410=DIRECTION('ref_axis',(1.,0.,0.));
#5411=DIRECTION('center_axis',(0.,0.,1.));
#5412=DIRECTION('ref_axis',(1.,0.,0.));
#5413=DIRECTION('center_axis',(0.,0.,1.));
#5414=DIRECTION('ref_axis',(1.,0.,0.));
#5415=DIRECTION('center_axis',(0.,0.,1.));
#5416=DIRECTION('ref_axis',(1.,0.,0.));
#5417=DIRECTION('',(0.,0.,1.));
#5418=DIRECTION('center_axis',(0.,0.,-1.));
#5419=DIRECTION('ref_axis',(1.,0.,0.));
#5420=DIRECTION('center_axis',(0.,0.,1.));
#5421=DIRECTION('ref_axis',(1.,0.,0.));
#5422=DIRECTION('center_axis',(0.,0.,1.));
#5423=DIRECTION('ref_axis',(1.,0.,0.));
#5424=DIRECTION('center_axis',(0.,0.,1.));
#5425=DIRECTION('ref_axis',(1.,0.,0.));
#5426=DIRECTION('',(0.,0.,1.));
#5427=DIRECTION('center_axis',(0.,0.,-1.));
#5428=DIRECTION('ref_axis',(1.,0.,0.));
#5429=DIRECTION('center_axis',(0.,0.,1.));
#5430=DIRECTION('ref_axis',(1.,0.,0.));
#5431=DIRECTION('center_axis',(0.,0.,1.));
#5432=DIRECTION('ref_axis',(1.,0.,0.));
#5433=DIRECTION('',(0.,0.,1.));
#5434=DIRECTION('center_axis',(0.,0.,-1.));
#5435=DIRECTION('ref_axis',(1.,0.,0.));
#5436=DIRECTION('center_axis',(0.,0.,1.));
#5437=DIRECTION('ref_axis',(1.,0.,0.));
#5438=DIRECTION('center_axis',(0.,0.,1.));
#5439=DIRECTION('ref_axis',(1.,0.,0.));
#5440=DIRECTION('',(0.,0.,1.));
#5441=DIRECTION('center_axis',(0.,0.,-1.));
#5442=DIRECTION('ref_axis',(1.,0.,0.));
#5443=DIRECTION('center_axis',(0.,0.,1.));
#5444=DIRECTION('ref_axis',(1.,0.,0.));
#5445=DIRECTION('center_axis',(0.,0.,1.));
#5446=DIRECTION('ref_axis',(1.,0.,0.));
#5447=DIRECTION('',(0.,0.,1.));
#5448=DIRECTION('center_axis',(0.,0.,-1.));
#5449=DIRECTION('ref_axis',(1.,0.,0.));
#5450=DIRECTION('center_axis',(0.,1.,0.));
#5451=DIRECTION('ref_axis',(-1.,0.,0.));
#5452=DIRECTION('',(-1.,0.,0.));
#5453=DIRECTION('',(0.,0.,1.));
#5454=DIRECTION('',(-1.,0.,0.));
#5455=DIRECTION('',(0.,0.,1.));
#5456=DIRECTION('center_axis',(1.,0.,0.));
#5457=DIRECTION('ref_axis',(0.,1.,0.));
#5458=DIRECTION('',(0.,1.,0.));
#5459=DIRECTION('',(0.,1.,0.));
#5460=DIRECTION('',(0.,0.,1.));
#5461=DIRECTION('center_axis',(0.,-1.,0.));
#5462=DIRECTION('ref_axis',(1.,0.,0.));
#5463=DIRECTION('',(1.,0.,0.));
#5464=DIRECTION('',(1.,0.,0.));
#5465=DIRECTION('',(0.,0.,1.));
#5466=DIRECTION('center_axis',(-1.,0.,0.));
#5467=DIRECTION('ref_axis',(0.,-1.,0.));
#5468=DIRECTION('',(0.,-1.,0.));
#5469=DIRECTION('',(0.,-1.,0.));
#5470=DIRECTION('center_axis',(0.,0.,1.));
#5471=DIRECTION('ref_axis',(1.,0.,0.));
#5472=DIRECTION('center_axis',(0.,0.,1.));
#5473=DIRECTION('ref_axis',(1.,0.,0.));
#5474=DIRECTION('axis',(0.,0.,1.));
#5475=DIRECTION('refdir',(1.,0.,0.));
#5476=DIRECTION('center_axis',(0.,1.,0.));
#5477=DIRECTION('ref_axis',(-1.,0.,0.));
#5478=DIRECTION('',(-1.,0.,0.));
#5479=DIRECTION('',(0.,0.,1.));
#5480=DIRECTION('',(-1.,0.,0.));
#5481=DIRECTION('',(0.,0.,1.));
#5482=DIRECTION('center_axis',(1.,0.,0.));
#5483=DIRECTION('ref_axis',(0.,1.,0.));
#5484=DIRECTION('',(0.,1.,0.));
#5485=DIRECTION('',(0.,1.,0.));
#5486=DIRECTION('',(0.,0.,1.));
#5487=DIRECTION('center_axis',(0.,-1.,0.));
#5488=DIRECTION('ref_axis',(1.,0.,0.));
#5489=DIRECTION('',(1.,0.,0.));
#5490=DIRECTION('',(1.,0.,0.));
#5491=DIRECTION('',(0.,0.,1.));
#5492=DIRECTION('center_axis',(-1.,0.,0.));
#5493=DIRECTION('ref_axis',(0.,-1.,0.));
#5494=DIRECTION('',(0.,-1.,0.));
#5495=DIRECTION('',(0.,-1.,0.));
#5496=DIRECTION('center_axis',(0.,0.,1.));
#5497=DIRECTION('ref_axis',(1.,0.,0.));
#5498=DIRECTION('center_axis',(0.,0.,1.));
#5499=DIRECTION('ref_axis',(1.,0.,0.));
#5500=DIRECTION('axis',(0.,0.,1.));
#5501=DIRECTION('refdir',(1.,0.,0.));
#5502=DIRECTION('center_axis',(0.,1.,0.));
#5503=DIRECTION('ref_axis',(-1.,0.,0.));
#5504=DIRECTION('',(-1.,0.,0.));
#5505=DIRECTION('',(0.,0.,1.));
#5506=DIRECTION('',(-1.,0.,0.));
#5507=DIRECTION('',(0.,0.,1.));
#5508=DIRECTION('center_axis',(1.,0.,0.));
#5509=DIRECTION('ref_axis',(0.,1.,0.));
#5510=DIRECTION('',(0.,1.,0.));
#5511=DIRECTION('',(0.,1.,0.));
#5512=DIRECTION('',(0.,0.,1.));
#5513=DIRECTION('center_axis',(0.,-1.,0.));
#5514=DIRECTION('ref_axis',(1.,0.,0.));
#5515=DIRECTION('',(1.,0.,0.));
#5516=DIRECTION('',(1.,0.,0.));
#5517=DIRECTION('',(0.,0.,1.));
#5518=DIRECTION('center_axis',(-1.,0.,0.));
#5519=DIRECTION('ref_axis',(0.,-1.,0.));
#5520=DIRECTION('',(0.,-1.,0.));
#5521=DIRECTION('',(0.,-1.,0.));
#5522=DIRECTION('center_axis',(0.,0.,1.));
#5523=DIRECTION('ref_axis',(1.,0.,0.));
#5524=DIRECTION('center_axis',(0.,0.,1.));
#5525=DIRECTION('ref_axis',(1.,0.,0.));
#5526=DIRECTION('axis',(0.,0.,1.));
#5527=DIRECTION('refdir',(1.,0.,0.));
#5528=DIRECTION('center_axis',(0.,0.,1.));
#5529=DIRECTION('ref_axis',(1.,0.,0.));
#5530=DIRECTION('center_axis',(0.,0.,1.));
#5531=DIRECTION('ref_axis',(1.,0.,0.));
#5532=DIRECTION('center_axis',(0.,0.,1.));
#5533=DIRECTION('ref_axis',(1.,0.,0.));
#5534=DIRECTION('center_axis',(0.,0.,1.));
#5535=DIRECTION('ref_axis',(0.78086880944303,0.624695047554425,0.));
#5536=DIRECTION('',(0.,0.,-1.));
#5537=DIRECTION('center_axis',(0.,0.,-1.));
#5538=DIRECTION('ref_axis',(1.,0.,0.));
#5539=DIRECTION('',(0.,0.,1.));
#5540=DIRECTION('center_axis',(0.,0.,1.));
#5541=DIRECTION('ref_axis',(1.,0.,0.));
#5542=DIRECTION('center_axis',(0.,0.,1.));
#5543=DIRECTION('ref_axis',(1.,0.,0.));
#5544=DIRECTION('center_axis',(0.,0.,1.));
#5545=DIRECTION('ref_axis',(1.,0.,0.));
#5546=DIRECTION('center_axis',(0.,0.,1.));
#5547=DIRECTION('ref_axis',(0.78086880944303,-0.624695047554425,0.));
#5548=DIRECTION('',(0.,0.,-1.));
#5549=DIRECTION('center_axis',(0.,0.,-1.));
#5550=DIRECTION('ref_axis',(1.,0.,0.));
#5551=DIRECTION('',(0.,0.,1.));
#5552=DIRECTION('center_axis',(0.,0.,1.));
#5553=DIRECTION('ref_axis',(1.,0.,0.));
#5554=DIRECTION('center_axis',(0.,0.,1.));
#5555=DIRECTION('ref_axis',(1.,0.,0.));
#5556=DIRECTION('',(0.,0.,1.));
#5557=DIRECTION('center_axis',(0.,0.,-1.));
#5558=DIRECTION('ref_axis',(1.,0.,0.));
#5559=DIRECTION('center_axis',(0.,0.,-1.));
#5560=DIRECTION('ref_axis',(1.,0.,0.));
#5561=DIRECTION('center_axis',(0.,0.,1.));
#5562=DIRECTION('ref_axis',(1.,0.,0.));
#5563=DIRECTION('center_axis',(0.,0.,1.));
#5564=DIRECTION('ref_axis',(1.,0.,0.));
#5565=DIRECTION('',(0.,0.,1.));
#5566=DIRECTION('center_axis',(0.,0.,-1.));
#5567=DIRECTION('ref_axis',(1.,0.,0.));
#5568=DIRECTION('center_axis',(0.,0.,-1.));
#5569=DIRECTION('ref_axis',(1.,0.,0.));
#5570=DIRECTION('center_axis',(0.,0.,1.));
#5571=DIRECTION('ref_axis',(1.,0.,0.));
#5572=DIRECTION('center_axis',(0.,0.,1.));
#5573=DIRECTION('ref_axis',(1.,0.,0.));
#5574=DIRECTION('',(0.,0.,1.));
#5575=DIRECTION('center_axis',(0.,0.,-1.));
#5576=DIRECTION('ref_axis',(1.,0.,0.));
#5577=DIRECTION('center_axis',(0.,0.,1.));
#5578=DIRECTION('ref_axis',(1.,0.,0.));
#5579=DIRECTION('center_axis',(0.,0.,1.));
#5580=DIRECTION('ref_axis',(1.,0.,0.));
#5581=DIRECTION('',(0.,0.,1.));
#5582=DIRECTION('center_axis',(0.,0.,-1.));
#5583=DIRECTION('ref_axis',(1.,0.,0.));
#5584=DIRECTION('center_axis',(0.,1.,0.));
#5585=DIRECTION('ref_axis',(-1.,0.,0.));
#5586=DIRECTION('',(-1.,0.,0.));
#5587=DIRECTION('',(0.,0.,1.));
#5588=DIRECTION('',(-1.,0.,0.));
#5589=DIRECTION('',(0.,0.,1.));
#5590=DIRECTION('center_axis',(1.,0.,0.));
#5591=DIRECTION('ref_axis',(0.,1.,0.));
#5592=DIRECTION('',(0.,1.,0.));
#5593=DIRECTION('',(0.,1.,0.));
#5594=DIRECTION('',(0.,0.,1.));
#5595=DIRECTION('center_axis',(0.,-1.,0.));
#5596=DIRECTION('ref_axis',(1.,0.,0.));
#5597=DIRECTION('',(1.,0.,0.));
#5598=DIRECTION('',(1.,0.,0.));
#5599=DIRECTION('',(0.,0.,1.));
#5600=DIRECTION('center_axis',(-1.,0.,0.));
#5601=DIRECTION('ref_axis',(0.,-1.,0.));
#5602=DIRECTION('',(0.,-1.,0.));
#5603=DIRECTION('',(0.,-1.,0.));
#5604=DIRECTION('center_axis',(0.,0.,1.));
#5605=DIRECTION('ref_axis',(1.,0.,0.));
#5606=DIRECTION('center_axis',(0.,0.,1.));
#5607=DIRECTION('ref_axis',(1.,0.,0.));
#5608=DIRECTION('axis',(0.,0.,1.));
#5609=DIRECTION('refdir',(1.,0.,0.));
#5610=DIRECTION('center_axis',(0.,0.,1.));
#5611=DIRECTION('ref_axis',(1.,0.,0.));
#5612=DIRECTION('center_axis',(0.,0.,1.));
#5613=DIRECTION('ref_axis',(1.,0.,0.));
#5614=DIRECTION('center_axis',(0.,0.,1.));
#5615=DIRECTION('ref_axis',(1.,0.,0.));
#5616=DIRECTION('center_axis',(0.,0.,1.));
#5617=DIRECTION('ref_axis',(-0.78086880944303,0.624695047554425,0.));
#5618=DIRECTION('',(0.,0.,-1.));
#5619=DIRECTION('center_axis',(0.,0.,-1.));
#5620=DIRECTION('ref_axis',(1.,0.,0.));
#5621=DIRECTION('',(0.,0.,1.));
#5622=DIRECTION('center_axis',(0.,0.,1.));
#5623=DIRECTION('ref_axis',(1.,0.,0.));
#5624=DIRECTION('center_axis',(0.,0.,1.));
#5625=DIRECTION('ref_axis',(1.,0.,0.));
#5626=DIRECTION('center_axis',(0.,0.,1.));
#5627=DIRECTION('ref_axis',(1.,0.,0.));
#5628=DIRECTION('center_axis',(0.,0.,1.));
#5629=DIRECTION('ref_axis',(-0.78086880944303,-0.624695047554425,0.));
#5630=DIRECTION('',(0.,0.,-1.));
#5631=DIRECTION('center_axis',(0.,0.,-1.));
#5632=DIRECTION('ref_axis',(1.,0.,0.));
#5633=DIRECTION('',(0.,0.,1.));
#5634=DIRECTION('center_axis',(0.,0.,1.));
#5635=DIRECTION('ref_axis',(1.,0.,0.));
#5636=DIRECTION('center_axis',(0.,0.,1.));
#5637=DIRECTION('ref_axis',(1.,0.,0.));
#5638=DIRECTION('',(0.,0.,1.));
#5639=DIRECTION('center_axis',(0.,0.,-1.));
#5640=DIRECTION('ref_axis',(1.,0.,0.));
#5641=DIRECTION('center_axis',(0.,0.,-1.));
#5642=DIRECTION('ref_axis',(1.,0.,0.));
#5643=DIRECTION('center_axis',(0.,0.,1.));
#5644=DIRECTION('ref_axis',(1.,0.,0.));
#5645=DIRECTION('center_axis',(0.,0.,1.));
#5646=DIRECTION('ref_axis',(1.,0.,0.));
#5647=DIRECTION('',(0.,0.,1.));
#5648=DIRECTION('center_axis',(0.,0.,-1.));
#5649=DIRECTION('ref_axis',(1.,0.,0.));
#5650=DIRECTION('center_axis',(0.,0.,-1.));
#5651=DIRECTION('ref_axis',(1.,0.,0.));
#5652=DIRECTION('center_axis',(0.,0.,1.));
#5653=DIRECTION('ref_axis',(1.,0.,0.));
#5654=DIRECTION('center_axis',(0.,0.,1.));
#5655=DIRECTION('ref_axis',(1.,0.,0.));
#5656=DIRECTION('',(0.,0.,1.));
#5657=DIRECTION('center_axis',(0.,0.,-1.));
#5658=DIRECTION('ref_axis',(1.,0.,0.));
#5659=DIRECTION('center_axis',(0.,0.,1.));
#5660=DIRECTION('ref_axis',(1.,0.,0.));
#5661=DIRECTION('center_axis',(0.,0.,1.));
#5662=DIRECTION('ref_axis',(1.,0.,0.));
#5663=DIRECTION('',(0.,0.,1.));
#5664=DIRECTION('center_axis',(0.,0.,-1.));
#5665=DIRECTION('ref_axis',(1.,0.,0.));
#5666=DIRECTION('center_axis',(0.,1.,0.));
#5667=DIRECTION('ref_axis',(-1.,0.,0.));
#5668=DIRECTION('',(-1.,0.,0.));
#5669=DIRECTION('',(0.,0.,1.));
#5670=DIRECTION('',(-1.,0.,0.));
#5671=DIRECTION('',(0.,0.,1.));
#5672=DIRECTION('center_axis',(1.,0.,0.));
#5673=DIRECTION('ref_axis',(0.,1.,0.));
#5674=DIRECTION('',(0.,1.,0.));
#5675=DIRECTION('',(0.,1.,0.));
#5676=DIRECTION('',(0.,0.,1.));
#5677=DIRECTION('center_axis',(0.,-1.,0.));
#5678=DIRECTION('ref_axis',(1.,0.,0.));
#5679=DIRECTION('',(1.,0.,0.));
#5680=DIRECTION('',(1.,0.,0.));
#5681=DIRECTION('',(0.,0.,1.));
#5682=DIRECTION('center_axis',(-1.,0.,0.));
#5683=DIRECTION('ref_axis',(0.,-1.,0.));
#5684=DIRECTION('',(0.,-1.,0.));
#5685=DIRECTION('',(0.,-1.,0.));
#5686=DIRECTION('center_axis',(0.,0.,1.));
#5687=DIRECTION('ref_axis',(1.,0.,0.));
#5688=DIRECTION('center_axis',(0.,0.,1.));
#5689=DIRECTION('ref_axis',(1.,0.,0.));
#5690=DIRECTION('axis',(0.,0.,1.));
#5691=DIRECTION('refdir',(1.,0.,0.));
#5692=DIRECTION('center_axis',(0.,0.,1.));
#5693=DIRECTION('ref_axis',(1.,0.,0.));
#5694=DIRECTION('center_axis',(0.,0.,1.));
#5695=DIRECTION('ref_axis',(1.,0.,0.));
#5696=DIRECTION('',(0.,0.,1.));
#5697=DIRECTION('center_axis',(0.,0.,-1.));
#5698=DIRECTION('ref_axis',(1.,0.,0.));
#5699=DIRECTION('center_axis',(0.,0.,1.));
#5700=DIRECTION('ref_axis',(1.,0.,0.));
#5701=DIRECTION('center_axis',(0.,0.,1.));
#5702=DIRECTION('ref_axis',(1.,0.,0.));
#5703=DIRECTION('',(0.,0.,1.));
#5704=DIRECTION('center_axis',(0.,0.,-1.));
#5705=DIRECTION('ref_axis',(1.,0.,0.));
#5706=DIRECTION('center_axis',(0.,0.,1.));
#5707=DIRECTION('ref_axis',(1.,0.,0.));
#5708=DIRECTION('center_axis',(0.,0.,1.));
#5709=DIRECTION('ref_axis',(1.,0.,0.));
#5710=DIRECTION('',(0.,0.,1.));
#5711=DIRECTION('center_axis',(0.,0.,-1.));
#5712=DIRECTION('ref_axis',(1.,0.,0.));
#5713=DIRECTION('center_axis',(0.,0.,1.));
#5714=DIRECTION('ref_axis',(1.,0.,0.));
#5715=DIRECTION('center_axis',(0.,0.,1.));
#5716=DIRECTION('ref_axis',(1.,0.,0.));
#5717=DIRECTION('',(0.,0.,1.));
#5718=DIRECTION('center_axis',(0.,0.,-1.));
#5719=DIRECTION('ref_axis',(1.,0.,0.));
#5720=DIRECTION('center_axis',(0.,0.,1.));
#5721=DIRECTION('ref_axis',(1.,0.,0.));
#5722=DIRECTION('center_axis',(0.,0.,1.));
#5723=DIRECTION('ref_axis',(1.,0.,0.));
#5724=DIRECTION('',(0.,0.,1.));
#5725=DIRECTION('center_axis',(0.,0.,-1.));
#5726=DIRECTION('ref_axis',(1.,0.,0.));
#5727=DIRECTION('center_axis',(0.,0.,1.));
#5728=DIRECTION('ref_axis',(1.,0.,0.));
#5729=DIRECTION('center_axis',(0.,0.,1.));
#5730=DIRECTION('ref_axis',(1.,0.,0.));
#5731=DIRECTION('',(0.,0.,1.));
#5732=DIRECTION('center_axis',(0.,0.,-1.));
#5733=DIRECTION('ref_axis',(1.,0.,0.));
#5734=DIRECTION('center_axis',(0.,0.,1.));
#5735=DIRECTION('ref_axis',(1.,0.,0.));
#5736=DIRECTION('center_axis',(0.,0.,1.));
#5737=DIRECTION('ref_axis',(1.,0.,0.));
#5738=DIRECTION('',(0.,0.,1.));
#5739=DIRECTION('center_axis',(0.,0.,-1.));
#5740=DIRECTION('ref_axis',(1.,0.,0.));
#5741=DIRECTION('center_axis',(0.,0.,1.));
#5742=DIRECTION('ref_axis',(1.,0.,0.));
#5743=DIRECTION('center_axis',(0.,0.,1.));
#5744=DIRECTION('ref_axis',(1.,0.,0.));
#5745=DIRECTION('',(0.,0.,1.));
#5746=DIRECTION('center_axis',(0.,0.,-1.));
#5747=DIRECTION('ref_axis',(1.,0.,0.));
#5748=DIRECTION('center_axis',(0.,0.,1.));
#5749=DIRECTION('ref_axis',(1.,0.,0.));
#5750=DIRECTION('center_axis',(0.,0.,1.));
#5751=DIRECTION('ref_axis',(1.,0.,0.));
#5752=DIRECTION('',(0.,0.,1.));
#5753=DIRECTION('center_axis',(0.,0.,-1.));
#5754=DIRECTION('ref_axis',(1.,0.,0.));
#5755=DIRECTION('center_axis',(0.,0.,1.));
#5756=DIRECTION('ref_axis',(1.,0.,0.));
#5757=DIRECTION('center_axis',(0.,0.,1.));
#5758=DIRECTION('ref_axis',(1.,0.,0.));
#5759=DIRECTION('',(0.,0.,1.));
#5760=DIRECTION('center_axis',(0.,0.,-1.));
#5761=DIRECTION('ref_axis',(1.,0.,0.));
#5762=DIRECTION('center_axis',(0.,0.,1.));
#5763=DIRECTION('ref_axis',(1.,0.,0.));
#5764=DIRECTION('center_axis',(0.,0.,1.));
#5765=DIRECTION('ref_axis',(1.,0.,0.));
#5766=DIRECTION('',(0.,0.,1.));
#5767=DIRECTION('center_axis',(0.,0.,-1.));
#5768=DIRECTION('ref_axis',(1.,0.,0.));
#5769=DIRECTION('center_axis',(0.,0.,1.));
#5770=DIRECTION('ref_axis',(1.,0.,0.));
#5771=DIRECTION('center_axis',(0.,0.,1.));
#5772=DIRECTION('ref_axis',(1.,0.,0.));
#5773=DIRECTION('',(0.,0.,1.));
#5774=DIRECTION('center_axis',(0.,0.,-1.));
#5775=DIRECTION('ref_axis',(1.,0.,0.));
#5776=DIRECTION('center_axis',(0.,1.,0.));
#5777=DIRECTION('ref_axis',(-1.,0.,0.));
#5778=DIRECTION('',(-1.,0.,0.));
#5779=DIRECTION('',(0.,0.,1.));
#5780=DIRECTION('',(-1.,0.,0.));
#5781=DIRECTION('',(0.,0.,1.));
#5782=DIRECTION('center_axis',(1.,0.,0.));
#5783=DIRECTION('ref_axis',(0.,1.,0.));
#5784=DIRECTION('',(0.,1.,0.));
#5785=DIRECTION('',(0.,1.,0.));
#5786=DIRECTION('',(0.,0.,1.));
#5787=DIRECTION('center_axis',(0.,-1.,0.));
#5788=DIRECTION('ref_axis',(1.,0.,0.));
#5789=DIRECTION('',(1.,0.,0.));
#5790=DIRECTION('',(1.,0.,0.));
#5791=DIRECTION('',(0.,0.,1.));
#5792=DIRECTION('center_axis',(-1.,0.,0.));
#5793=DIRECTION('ref_axis',(0.,-1.,0.));
#5794=DIRECTION('',(0.,-1.,0.));
#5795=DIRECTION('',(0.,-1.,0.));
#5796=DIRECTION('center_axis',(0.,0.,1.));
#5797=DIRECTION('ref_axis',(1.,0.,0.));
#5798=DIRECTION('center_axis',(0.,0.,1.));
#5799=DIRECTION('ref_axis',(1.,0.,0.));
#5800=DIRECTION('axis',(0.,0.,1.));
#5801=DIRECTION('refdir',(1.,0.,0.));
#5802=DIRECTION('center_axis',(0.,0.,1.));
#5803=DIRECTION('ref_axis',(1.,0.,0.));
#5804=DIRECTION('center_axis',(0.,0.,1.));
#5805=DIRECTION('ref_axis',(1.,0.,0.));
#5806=DIRECTION('',(0.,0.,1.));
#5807=DIRECTION('center_axis',(0.,0.,-1.));
#5808=DIRECTION('ref_axis',(1.,0.,0.));
#5809=DIRECTION('center_axis',(0.,0.,1.));
#5810=DIRECTION('ref_axis',(1.,0.,0.));
#5811=DIRECTION('center_axis',(0.,0.,1.));
#5812=DIRECTION('ref_axis',(1.,0.,0.));
#5813=DIRECTION('',(0.,0.,1.));
#5814=DIRECTION('center_axis',(0.,0.,-1.));
#5815=DIRECTION('ref_axis',(1.,0.,0.));
#5816=DIRECTION('center_axis',(0.,0.,1.));
#5817=DIRECTION('ref_axis',(1.,0.,0.));
#5818=DIRECTION('center_axis',(0.,0.,1.));
#5819=DIRECTION('ref_axis',(1.,0.,0.));
#5820=DIRECTION('',(0.,0.,1.));
#5821=DIRECTION('center_axis',(0.,0.,-1.));
#5822=DIRECTION('ref_axis',(1.,0.,0.));
#5823=DIRECTION('center_axis',(0.,0.,1.));
#5824=DIRECTION('ref_axis',(1.,0.,0.));
#5825=DIRECTION('center_axis',(0.,0.,1.));
#5826=DIRECTION('ref_axis',(1.,0.,0.));
#5827=DIRECTION('',(0.,0.,1.));
#5828=DIRECTION('center_axis',(0.,0.,-1.));
#5829=DIRECTION('ref_axis',(1.,0.,0.));
#5830=DIRECTION('center_axis',(0.,0.,1.));
#5831=DIRECTION('ref_axis',(1.,0.,0.));
#5832=DIRECTION('center_axis',(0.,0.,1.));
#5833=DIRECTION('ref_axis',(1.,0.,0.));
#5834=DIRECTION('',(0.,0.,1.));
#5835=DIRECTION('center_axis',(0.,0.,-1.));
#5836=DIRECTION('ref_axis',(1.,0.,0.));
#5837=DIRECTION('center_axis',(0.,0.,1.));
#5838=DIRECTION('ref_axis',(1.,0.,0.));
#5839=DIRECTION('center_axis',(0.,0.,1.));
#5840=DIRECTION('ref_axis',(1.,0.,0.));
#5841=DIRECTION('',(0.,0.,1.));
#5842=DIRECTION('center_axis',(0.,0.,-1.));
#5843=DIRECTION('ref_axis',(1.,0.,0.));
#5844=DIRECTION('center_axis',(0.,0.,1.));
#5845=DIRECTION('ref_axis',(1.,0.,0.));
#5846=DIRECTION('center_axis',(0.,0.,1.));
#5847=DIRECTION('ref_axis',(1.,0.,0.));
#5848=DIRECTION('',(0.,0.,1.));
#5849=DIRECTION('center_axis',(0.,0.,-1.));
#5850=DIRECTION('ref_axis',(1.,0.,0.));
#5851=DIRECTION('center_axis',(0.,0.,1.));
#5852=DIRECTION('ref_axis',(1.,0.,0.));
#5853=DIRECTION('center_axis',(0.,0.,1.));
#5854=DIRECTION('ref_axis',(1.,0.,0.));
#5855=DIRECTION('',(0.,0.,1.));
#5856=DIRECTION('center_axis',(0.,0.,-1.));
#5857=DIRECTION('ref_axis',(1.,0.,0.));
#5858=DIRECTION('center_axis',(0.,-1.,0.));
#5859=DIRECTION('ref_axis',(1.,0.,0.));
#5860=DIRECTION('',(-1.,0.,0.));
#5861=DIRECTION('',(0.,0.,1.));
#5862=DIRECTION('',(1.,0.,0.));
#5863=DIRECTION('',(0.,0.,1.));
#5864=DIRECTION('center_axis',(-1.,0.,0.));
#5865=DIRECTION('ref_axis',(0.,-1.,0.));
#5866=DIRECTION('',(0.,1.,0.));
#5867=DIRECTION('',(0.,-1.,0.));
#5868=DIRECTION('',(0.,0.,1.));
#5869=DIRECTION('center_axis',(0.,1.,0.));
#5870=DIRECTION('ref_axis',(-1.,0.,0.));
#5871=DIRECTION('',(1.,0.,0.));
#5872=DIRECTION('',(-1.,0.,0.));
#5873=DIRECTION('',(0.,0.,1.));
#5874=DIRECTION('center_axis',(1.,0.,0.));
#5875=DIRECTION('ref_axis',(0.,1.,0.));
#5876=DIRECTION('',(0.,-1.,0.));
#5877=DIRECTION('',(0.,1.,0.));
#5878=DIRECTION('center_axis',(0.,1.,0.));
#5879=DIRECTION('ref_axis',(-1.,0.,0.));
#5880=DIRECTION('',(-1.,0.,0.));
#5881=DIRECTION('',(0.,0.,1.));
#5882=DIRECTION('',(-1.,0.,0.));
#5883=DIRECTION('',(0.,0.,1.));
#5884=DIRECTION('center_axis',(1.,0.,0.));
#5885=DIRECTION('ref_axis',(0.,1.,0.));
#5886=DIRECTION('',(0.,1.,0.));
#5887=DIRECTION('',(0.,1.,0.));
#5888=DIRECTION('',(0.,0.,1.));
#5889=DIRECTION('center_axis',(0.,-1.,0.));
#5890=DIRECTION('ref_axis',(1.,0.,0.));
#5891=DIRECTION('',(1.,0.,0.));
#5892=DIRECTION('',(1.,0.,0.));
#5893=DIRECTION('',(0.,0.,1.));
#5894=DIRECTION('center_axis',(-1.,0.,0.));
#5895=DIRECTION('ref_axis',(0.,-1.,0.));
#5896=DIRECTION('',(0.,-1.,0.));
#5897=DIRECTION('',(0.,-1.,0.));
#5898=DIRECTION('center_axis',(0.,0.,1.));
#5899=DIRECTION('ref_axis',(1.,0.,0.));
#5900=DIRECTION('center_axis',(0.,0.,1.));
#5901=DIRECTION('ref_axis',(1.,0.,0.));
#5902=DIRECTION('axis',(0.,0.,1.));
#5903=DIRECTION('refdir',(1.,0.,0.));
#5904=DIRECTION('center_axis',(0.,1.,0.));
#5905=DIRECTION('ref_axis',(1.,0.,0.));
#5906=DIRECTION('center_axis',(0.,1.,0.));
#5907=DIRECTION('ref_axis',(1.,0.,0.));
#5908=DIRECTION('',(0.,1.,0.));
#5909=DIRECTION('center_axis',(0.,1.,0.));
#5910=DIRECTION('ref_axis',(1.,0.,0.));
#5911=DIRECTION('center_axis',(0.,1.,0.));
#5912=DIRECTION('ref_axis',(1.,0.,0.));
#5913=DIRECTION('center_axis',(0.,1.,0.));
#5914=DIRECTION('ref_axis',(1.,0.,0.));
#5915=DIRECTION('center_axis',(0.,1.,0.));
#5916=DIRECTION('ref_axis',(1.,0.,0.));
#5917=DIRECTION('',(0.,1.,0.));
#5918=DIRECTION('center_axis',(0.,1.,0.));
#5919=DIRECTION('ref_axis',(1.,0.,0.));
#5920=DIRECTION('center_axis',(0.,1.,0.));
#5921=DIRECTION('ref_axis',(1.,0.,0.));
#5922=DIRECTION('center_axis',(0.,0.,1.));
#5923=DIRECTION('ref_axis',(1.,0.,0.));
#5924=DIRECTION('center_axis',(0.,0.,1.));
#5925=DIRECTION('ref_axis',(1.,0.,0.));
#5926=DIRECTION('',(0.,0.,1.));
#5927=DIRECTION('center_axis',(0.,0.,1.));
#5928=DIRECTION('ref_axis',(1.,0.,0.));
#5929=DIRECTION('center_axis',(0.,0.,1.));
#5930=DIRECTION('ref_axis',(1.,0.,0.));
#5931=DIRECTION('center_axis',(0.,0.,1.));
#5932=DIRECTION('ref_axis',(1.,0.,0.));
#5933=DIRECTION('center_axis',(0.,0.,1.));
#5934=DIRECTION('ref_axis',(1.,0.,0.));
#5935=DIRECTION('',(0.,0.,1.));
#5936=DIRECTION('center_axis',(0.,0.,1.));
#5937=DIRECTION('ref_axis',(1.,0.,0.));
#5938=DIRECTION('center_axis',(0.,0.,1.));
#5939=DIRECTION('ref_axis',(1.,0.,0.));
#5940=DIRECTION('center_axis',(0.,0.,1.));
#5941=DIRECTION('ref_axis',(1.,0.,0.));
#5942=DIRECTION('center_axis',(0.,0.,1.));
#5943=DIRECTION('ref_axis',(1.,0.,0.));
#5944=DIRECTION('',(0.,0.,1.));
#5945=DIRECTION('center_axis',(0.,0.,1.));
#5946=DIRECTION('ref_axis',(1.,0.,0.));
#5947=DIRECTION('center_axis',(0.,0.,1.));
#5948=DIRECTION('ref_axis',(1.,0.,0.));
#5949=DIRECTION('center_axis',(0.,0.,1.));
#5950=DIRECTION('ref_axis',(1.,0.,0.));
#5951=DIRECTION('center_axis',(0.,0.,1.));
#5952=DIRECTION('ref_axis',(1.,0.,0.));
#5953=DIRECTION('',(0.,0.,1.));
#5954=DIRECTION('center_axis',(0.,0.,1.));
#5955=DIRECTION('ref_axis',(1.,0.,0.));
#5956=DIRECTION('center_axis',(0.,0.,1.));
#5957=DIRECTION('ref_axis',(1.,0.,0.));
#5958=DIRECTION('center_axis',(0.,0.,1.));
#5959=DIRECTION('ref_axis',(1.,0.,0.));
#5960=DIRECTION('center_axis',(0.,0.,1.));
#5961=DIRECTION('ref_axis',(1.,0.,0.));
#5962=DIRECTION('',(0.,0.,1.));
#5963=DIRECTION('center_axis',(0.,0.,1.));
#5964=DIRECTION('ref_axis',(1.,0.,0.));
#5965=DIRECTION('center_axis',(0.,0.,1.));
#5966=DIRECTION('ref_axis',(1.,0.,0.));
#5967=DIRECTION('center_axis',(0.,0.,1.));
#5968=DIRECTION('ref_axis',(1.,0.,0.));
#5969=DIRECTION('center_axis',(0.,0.,1.));
#5970=DIRECTION('ref_axis',(1.,0.,0.));
#5971=DIRECTION('',(0.,0.,1.));
#5972=DIRECTION('center_axis',(0.,0.,1.));
#5973=DIRECTION('ref_axis',(1.,0.,0.));
#5974=DIRECTION('center_axis',(0.,0.,1.));
#5975=DIRECTION('ref_axis',(1.,0.,0.));
#5976=DIRECTION('center_axis',(0.,0.,1.));
#5977=DIRECTION('ref_axis',(1.,0.,0.));
#5978=DIRECTION('center_axis',(0.,0.,1.));
#5979=DIRECTION('ref_axis',(1.,0.,0.));
#5980=DIRECTION('',(0.,0.,1.));
#5981=DIRECTION('center_axis',(0.,0.,1.));
#5982=DIRECTION('ref_axis',(1.,0.,0.));
#5983=DIRECTION('center_axis',(0.,0.,1.));
#5984=DIRECTION('ref_axis',(1.,0.,0.));
#5985=DIRECTION('center_axis',(0.,0.,1.));
#5986=DIRECTION('ref_axis',(1.,0.,0.));
#5987=DIRECTION('center_axis',(0.,0.,1.));
#5988=DIRECTION('ref_axis',(1.,0.,0.));
#5989=DIRECTION('',(0.,0.,1.));
#5990=DIRECTION('center_axis',(0.,0.,1.));
#5991=DIRECTION('ref_axis',(1.,0.,0.));
#5992=DIRECTION('center_axis',(0.,0.,1.));
#5993=DIRECTION('ref_axis',(1.,0.,0.));
#5994=DIRECTION('center_axis',(1.,0.,0.));
#5995=DIRECTION('ref_axis',(0.,0.,-1.));
#5996=DIRECTION('center_axis',(1.,0.,0.));
#5997=DIRECTION('ref_axis',(0.,0.,-1.));
#5998=DIRECTION('',(1.,0.,0.));
#5999=DIRECTION('center_axis',(-1.,0.,0.));
#6000=DIRECTION('ref_axis',(0.,0.,-1.));
#6001=DIRECTION('center_axis',(1.,0.,0.));
#6002=DIRECTION('ref_axis',(0.,0.,-1.));
#6003=DIRECTION('center_axis',(1.,0.,0.));
#6004=DIRECTION('ref_axis',(0.,0.,-1.));
#6005=DIRECTION('center_axis',(1.,0.,0.));
#6006=DIRECTION('ref_axis',(0.,0.,-1.));
#6007=DIRECTION('center_axis',(1.,0.,0.));
#6008=DIRECTION('ref_axis',(0.,0.,-1.));
#6009=DIRECTION('',(1.,0.,0.));
#6010=DIRECTION('center_axis',(1.,0.,0.));
#6011=DIRECTION('ref_axis',(0.,0.,-1.));
#6012=DIRECTION('center_axis',(1.,0.,0.));
#6013=DIRECTION('ref_axis',(0.,0.,-1.));
#6014=DIRECTION('center_axis',(-1.,0.,0.));
#6015=DIRECTION('ref_axis',(0.,0.,-1.));
#6016=DIRECTION('center_axis',(0.,0.,1.));
#6017=DIRECTION('ref_axis',(1.,0.,0.));
#6018=DIRECTION('',(0.,0.,1.));
#6019=DIRECTION('center_axis',(0.,0.,-1.));
#6020=DIRECTION('ref_axis',(1.,0.,0.));
#6021=DIRECTION('center_axis',(0.,0.,1.));
#6022=DIRECTION('ref_axis',(1.,0.,0.));
#6023=DIRECTION('center_axis',(0.,0.,1.));
#6024=DIRECTION('ref_axis',(1.,0.,0.));
#6025=DIRECTION('',(0.,0.,1.));
#6026=DIRECTION('center_axis',(0.,0.,-1.));
#6027=DIRECTION('ref_axis',(1.,0.,0.));
#6028=DIRECTION('center_axis',(0.,0.,1.));
#6029=DIRECTION('ref_axis',(1.,0.,0.));
#6030=DIRECTION('center_axis',(0.,0.,1.));
#6031=DIRECTION('ref_axis',(1.,0.,0.));
#6032=DIRECTION('',(0.,0.,1.));
#6033=DIRECTION('center_axis',(0.,0.,-1.));
#6034=DIRECTION('ref_axis',(1.,0.,0.));
#6035=DIRECTION('center_axis',(0.,0.,1.));
#6036=DIRECTION('ref_axis',(1.,0.,0.));
#6037=DIRECTION('center_axis',(0.,0.,1.));
#6038=DIRECTION('ref_axis',(1.,0.,0.));
#6039=DIRECTION('',(0.,0.,1.));
#6040=DIRECTION('center_axis',(0.,0.,-1.));
#6041=DIRECTION('ref_axis',(1.,0.,0.));
#6042=DIRECTION('center_axis',(0.,0.,1.));
#6043=DIRECTION('ref_axis',(1.,0.,0.));
#6044=DIRECTION('center_axis',(0.,0.,1.));
#6045=DIRECTION('ref_axis',(1.,0.,0.));
#6046=DIRECTION('',(0.,0.,1.));
#6047=DIRECTION('center_axis',(0.,0.,-1.));
#6048=DIRECTION('ref_axis',(1.,0.,0.));
#6049=DIRECTION('center_axis',(0.,0.,1.));
#6050=DIRECTION('ref_axis',(1.,0.,0.));
#6051=DIRECTION('center_axis',(0.,0.,1.));
#6052=DIRECTION('ref_axis',(1.,0.,0.));
#6053=DIRECTION('',(0.,0.,1.));
#6054=DIRECTION('center_axis',(0.,0.,-1.));
#6055=DIRECTION('ref_axis',(1.,0.,0.));
#6056=DIRECTION('center_axis',(0.,0.,1.));
#6057=DIRECTION('ref_axis',(1.,0.,0.));
#6058=DIRECTION('center_axis',(0.,0.,1.));
#6059=DIRECTION('ref_axis',(1.,0.,0.));
#6060=DIRECTION('',(0.,0.,1.));
#6061=DIRECTION('center_axis',(0.,0.,-1.));
#6062=DIRECTION('ref_axis',(1.,0.,0.));
#6063=DIRECTION('center_axis',(0.,0.,1.));
#6064=DIRECTION('ref_axis',(1.,0.,0.));
#6065=DIRECTION('center_axis',(0.,0.,1.));
#6066=DIRECTION('ref_axis',(1.,0.,0.));
#6067=DIRECTION('',(0.,0.,1.));
#6068=DIRECTION('center_axis',(0.,0.,-1.));
#6069=DIRECTION('ref_axis',(1.,0.,0.));
#6070=DIRECTION('center_axis',(0.,0.,1.));
#6071=DIRECTION('ref_axis',(1.,0.,0.));
#6072=DIRECTION('center_axis',(0.,-1.,0.));
#6073=DIRECTION('ref_axis',(1.,0.,0.));
#6074=DIRECTION('',(1.,0.,0.));
#6075=DIRECTION('',(0.,0.,1.));
#6076=DIRECTION('',(1.,0.,0.));
#6077=DIRECTION('',(0.,0.,1.));
#6078=DIRECTION('center_axis',(1.,0.,0.));
#6079=DIRECTION('ref_axis',(0.,1.,0.));
#6080=DIRECTION('',(0.,1.,0.));
#6081=DIRECTION('',(0.,1.,0.));
#6082=DIRECTION('center_axis',(-1.,0.,0.));
#6083=DIRECTION('ref_axis',(0.,0.,-1.));
#6084=DIRECTION('',(0.,1.,0.));
#6085=DIRECTION('',(0.,0.,1.));
#6086=DIRECTION('center_axis',(0.,0.,1.));
#6087=DIRECTION('ref_axis',(1.,0.,0.));
#6088=DIRECTION('',(-1.,0.,0.));
#6089=DIRECTION('',(0.,-1.,0.));
#6090=DIRECTION('center_axis',(0.,1.,0.));
#6091=DIRECTION('ref_axis',(-1.,0.,0.));
#6092=DIRECTION('',(-1.,0.,0.));
#6093=DIRECTION('',(-1.,0.,0.));
#6094=DIRECTION('',(0.,0.,1.));
#6095=DIRECTION('center_axis',(-1.,0.,0.));
#6096=DIRECTION('ref_axis',(0.,-1.,0.));
#6097=DIRECTION('',(0.,-1.,0.));
#6098=DIRECTION('',(0.,-1.,0.));
#6099=DIRECTION('center_axis',(1.,0.,0.));
#6100=DIRECTION('ref_axis',(0.,0.,-1.));
#6101=DIRECTION('center_axis',(0.,0.,1.));
#6102=DIRECTION('ref_axis',(1.,0.,0.));
#6103=DIRECTION('',(1.,0.,0.));
#6104=DIRECTION('center_axis',(1.,0.,0.));
#6105=DIRECTION('ref_axis',(0.,0.,-1.));
#6106=DIRECTION('',(1.,0.,0.));
#6107=DIRECTION('',(1.,0.,0.));
#6108=DIRECTION('',(1.,0.,0.));
#6109=DIRECTION('',(1.,0.,0.));
#6110=DIRECTION('',(1.,0.,0.));
#6111=DIRECTION('center_axis',(0.,1.,0.));
#6112=DIRECTION('ref_axis',(-1.,0.,0.));
#6113=DIRECTION('',(-1.,0.,0.));
#6114=DIRECTION('',(0.,0.,1.));
#6115=DIRECTION('',(-1.,0.,0.));
#6116=DIRECTION('',(0.,0.,1.));
#6117=DIRECTION('center_axis',(1.,0.,0.));
#6118=DIRECTION('ref_axis',(0.,1.,0.));
#6119=DIRECTION('',(0.,1.,0.));
#6120=DIRECTION('',(0.,1.,0.));
#6121=DIRECTION('',(0.,0.,1.));
#6122=DIRECTION('center_axis',(0.,-1.,0.));
#6123=DIRECTION('ref_axis',(1.,0.,0.));
#6124=DIRECTION('',(1.,0.,0.));
#6125=DIRECTION('',(1.,0.,0.));
#6126=DIRECTION('',(0.,0.,1.));
#6127=DIRECTION('center_axis',(-1.,0.,0.));
#6128=DIRECTION('ref_axis',(0.,-1.,0.));
#6129=DIRECTION('',(0.,-1.,0.));
#6130=DIRECTION('',(0.,-1.,0.));
#6131=DIRECTION('center_axis',(0.,0.,1.));
#6132=DIRECTION('ref_axis',(1.,0.,0.));
#6133=DIRECTION('center_axis',(0.,0.,1.));
#6134=DIRECTION('ref_axis',(1.,0.,0.));
#6135=DIRECTION('axis',(0.,0.,1.));
#6136=DIRECTION('refdir',(1.,0.,0.));
#6137=DIRECTION('center_axis',(0.,0.,1.));
#6138=DIRECTION('ref_axis',(1.,0.,0.));
#6139=DIRECTION('center_axis',(0.,0.,-1.));
#6140=DIRECTION('ref_axis',(1.,0.,0.));
#6141=DIRECTION('',(0.,0.,-1.));
#6142=DIRECTION('center_axis',(0.,0.,-1.));
#6143=DIRECTION('ref_axis',(1.,0.,0.));
#6144=DIRECTION('center_axis',(0.,0.,1.));
#6145=DIRECTION('ref_axis',(1.,0.,0.));
#6146=DIRECTION('center_axis',(0.,0.,1.));
#6147=DIRECTION('ref_axis',(1.,0.,0.));
#6148=DIRECTION('',(0.,0.,-1.));
#6149=DIRECTION('center_axis',(0.,0.,1.));
#6150=DIRECTION('ref_axis',(1.,0.,0.));
#6151=DIRECTION('center_axis',(0.,0.,1.));
#6152=DIRECTION('ref_axis',(1.,0.,0.));
#6153=DIRECTION('center_axis',(0.,0.,1.));
#6154=DIRECTION('ref_axis',(1.,0.,0.));
#6155=DIRECTION('axis',(0.,0.,1.));
#6156=DIRECTION('refdir',(1.,0.,0.));
#6157=DIRECTION('center_axis',(0.,0.,1.));
#6158=DIRECTION('ref_axis',(1.,0.,0.));
#6159=DIRECTION('center_axis',(0.,0.,-1.));
#6160=DIRECTION('ref_axis',(1.,0.,0.));
#6161=DIRECTION('',(0.,0.,-1.));
#6162=DIRECTION('center_axis',(0.,0.,-1.));
#6163=DIRECTION('ref_axis',(1.,0.,0.));
#6164=DIRECTION('center_axis',(0.,0.,1.));
#6165=DIRECTION('ref_axis',(1.,0.,0.));
#6166=DIRECTION('center_axis',(0.,0.,1.));
#6167=DIRECTION('ref_axis',(1.,0.,0.));
#6168=DIRECTION('',(0.,0.,-1.));
#6169=DIRECTION('center_axis',(0.,0.,1.));
#6170=DIRECTION('ref_axis',(1.,0.,0.));
#6171=DIRECTION('center_axis',(0.,0.,1.));
#6172=DIRECTION('ref_axis',(1.,0.,0.));
#6173=DIRECTION('center_axis',(0.,0.,1.));
#6174=DIRECTION('ref_axis',(1.,0.,0.));
#6175=DIRECTION('axis',(0.,0.,1.));
#6176=DIRECTION('refdir',(1.,0.,0.));
#6177=DIRECTION('center_axis',(0.,0.,1.));
#6178=DIRECTION('ref_axis',(1.,0.,0.));
#6179=DIRECTION('center_axis',(0.,0.,-1.));
#6180=DIRECTION('ref_axis',(1.,0.,0.));
#6181=DIRECTION('',(0.,0.,-1.));
#6182=DIRECTION('center_axis',(0.,0.,-1.));
#6183=DIRECTION('ref_axis',(1.,0.,0.));
#6184=DIRECTION('center_axis',(0.,0.,1.));
#6185=DIRECTION('ref_axis',(1.,0.,0.));
#6186=DIRECTION('center_axis',(0.,0.,1.));
#6187=DIRECTION('ref_axis',(1.,0.,0.));
#6188=DIRECTION('',(0.,0.,-1.));
#6189=DIRECTION('center_axis',(0.,0.,1.));
#6190=DIRECTION('ref_axis',(1.,0.,0.));
#6191=DIRECTION('center_axis',(0.,0.,1.));
#6192=DIRECTION('ref_axis',(1.,0.,0.));
#6193=DIRECTION('center_axis',(0.,0.,1.));
#6194=DIRECTION('ref_axis',(1.,0.,0.));
#6195=DIRECTION('axis',(0.,0.,1.));
#6196=DIRECTION('refdir',(1.,0.,0.));
#6197=DIRECTION('center_axis',(0.,0.,1.));
#6198=DIRECTION('ref_axis',(1.,0.,0.));
#6199=DIRECTION('center_axis',(0.,0.,-1.));
#6200=DIRECTION('ref_axis',(1.,0.,0.));
#6201=DIRECTION('',(0.,0.,-1.));
#6202=DIRECTION('center_axis',(0.,0.,-1.));
#6203=DIRECTION('ref_axis',(1.,0.,0.));
#6204=DIRECTION('center_axis',(0.,0.,1.));
#6205=DIRECTION('ref_axis',(1.,0.,0.));
#6206=DIRECTION('center_axis',(0.,0.,1.));
#6207=DIRECTION('ref_axis',(1.,0.,0.));
#6208=DIRECTION('',(0.,0.,-1.));
#6209=DIRECTION('center_axis',(0.,0.,1.));
#6210=DIRECTION('ref_axis',(1.,0.,0.));
#6211=DIRECTION('center_axis',(0.,0.,1.));
#6212=DIRECTION('ref_axis',(1.,0.,0.));
#6213=DIRECTION('center_axis',(0.,0.,1.));
#6214=DIRECTION('ref_axis',(1.,0.,0.));
#6215=DIRECTION('axis',(0.,0.,1.));
#6216=DIRECTION('refdir',(1.,0.,0.));
#6217=DIRECTION('center_axis',(1.,0.,0.));
#6218=DIRECTION('ref_axis',(0.,0.,-1.));
#6219=DIRECTION('',(0.,0.5,0.866025403784439));
#6220=DIRECTION('',(0.,1.,-4.39534328316243E-16));
#6221=DIRECTION('',(0.,0.5,-0.866025403784439));
#6222=DIRECTION('',(0.,-0.5,-0.866025403784439));
#6223=DIRECTION('',(0.,-1.,0.));
#6224=DIRECTION('',(0.,-0.5,0.866025403784439));
#6225=DIRECTION('center_axis',(1.,0.,0.));
#6226=DIRECTION('ref_axis',(0.,0.,-1.));
#6227=DIRECTION('center_axis',(0.,-4.39534328316243E-16,-1.));
#6228=DIRECTION('ref_axis',(0.,1.,-4.39534328316243E-16));
#6229=DIRECTION('',(1.,0.,0.));
#6230=DIRECTION('',(0.,1.,-4.39534328316243E-16));
#6231=DIRECTION('',(1.,0.,0.));
#6232=DIRECTION('center_axis',(0.,-0.866025403784439,-0.5));
#6233=DIRECTION('ref_axis',(0.,0.5,-0.866025403784439));
#6234=DIRECTION('',(0.,0.5,-0.866025403784439));
#6235=DIRECTION('',(1.,0.,0.));
#6236=DIRECTION('center_axis',(0.,-0.866025403784439,0.5));
#6237=DIRECTION('ref_axis',(0.,-0.5,-0.866025403784439));
#6238=DIRECTION('',(0.,-0.5,-0.866025403784439));
#6239=DIRECTION('',(1.,0.,0.));
#6240=DIRECTION('center_axis',(0.,0.,1.));
#6241=DIRECTION('ref_axis',(0.,-1.,0.));
#6242=DIRECTION('',(0.,-1.,0.));
#6243=DIRECTION('',(1.,0.,0.));
#6244=DIRECTION('center_axis',(0.,0.866025403784439,0.5));
#6245=DIRECTION('ref_axis',(0.,-0.5,0.866025403784439));
#6246=DIRECTION('',(0.,-0.5,0.866025403784439));
#6247=DIRECTION('',(1.,0.,0.));
#6248=DIRECTION('center_axis',(0.,0.866025403784439,-0.5));
#6249=DIRECTION('ref_axis',(0.,0.5,0.866025403784439));
#6250=DIRECTION('',(0.,0.5,0.866025403784439));
#6251=DIRECTION('center_axis',(1.,0.,0.));
#6252=DIRECTION('ref_axis',(0.,0.,-1.));
#6253=DIRECTION('center_axis',(1.,0.,0.));
#6254=DIRECTION('ref_axis',(0.,0.,-1.));
#6255=DIRECTION('',(-1.,0.,0.));
#6256=DIRECTION('center_axis',(1.,0.,0.));
#6257=DIRECTION('ref_axis',(0.,0.,-1.));
#6258=DIRECTION('center_axis',(1.,0.,0.));
#6259=DIRECTION('ref_axis',(0.,0.,-1.));
#6260=DIRECTION('axis',(0.,0.,1.));
#6261=DIRECTION('refdir',(1.,0.,0.));
#6262=DIRECTION('center_axis',(0.,0.,1.));
#6263=DIRECTION('ref_axis',(1.,0.,0.));
#6264=DIRECTION('center_axis',(0.,0.,1.));
#6265=DIRECTION('ref_axis',(1.,0.,0.));
#6266=DIRECTION('',(0.,0.,-1.));
#6267=DIRECTION('center_axis',(0.,0.,1.));
#6268=DIRECTION('ref_axis',(1.,0.,0.));
#6269=DIRECTION('center_axis',(0.,0.,1.));
#6270=DIRECTION('ref_axis',(1.,0.,0.));
#6271=DIRECTION('center_axis',(0.,0.,1.));
#6272=DIRECTION('ref_axis',(1.,0.,0.));
#6273=DIRECTION('axis',(0.,0.,1.));
#6274=DIRECTION('refdir',(1.,0.,0.));
#6275=DIRECTION('center_axis',(0.,0.,1.));
#6276=DIRECTION('ref_axis',(1.,0.,0.));
#6277=DIRECTION('center_axis',(0.,0.,1.));
#6278=DIRECTION('ref_axis',(1.,0.,0.));
#6279=DIRECTION('',(0.,0.,-1.));
#6280=DIRECTION('center_axis',(0.,0.,1.));
#6281=DIRECTION('ref_axis',(1.,0.,0.));
#6282=DIRECTION('center_axis',(0.,0.,1.));
#6283=DIRECTION('ref_axis',(1.,0.,0.));
#6284=DIRECTION('center_axis',(0.,0.,1.));
#6285=DIRECTION('ref_axis',(1.,0.,0.));
#6286=DIRECTION('axis',(0.,0.,1.));
#6287=DIRECTION('refdir',(1.,0.,0.));
#6288=DIRECTION('center_axis',(0.,1.,0.));
#6289=DIRECTION('ref_axis',(1.,0.,0.));
#6290=DIRECTION('center_axis',(0.,1.,0.));
#6291=DIRECTION('ref_axis',(1.,0.,0.));
#6292=DIRECTION('',(0.,1.,0.));
#6293=DIRECTION('center_axis',(0.,-1.,0.));
#6294=DIRECTION('ref_axis',(1.,0.,0.));
#6295=DIRECTION('center_axis',(0.,1.,0.));
#6296=DIRECTION('ref_axis',(1.,0.,0.));
#6297=DIRECTION('center_axis',(0.,1.,0.));
#6298=DIRECTION('ref_axis',(1.,0.,0.));
#6299=DIRECTION('',(0.,1.,0.));
#6300=DIRECTION('center_axis',(0.,-1.,0.));
#6301=DIRECTION('ref_axis',(1.,0.,0.));
#6302=DIRECTION('center_axis',(0.,1.,0.));
#6303=DIRECTION('ref_axis',(-1.,0.,0.));
#6304=DIRECTION('',(-1.,0.,0.));
#6305=DIRECTION('',(0.,0.,1.));
#6306=DIRECTION('',(-1.,0.,0.));
#6307=DIRECTION('',(0.,0.,1.));
#6308=DIRECTION('center_axis',(1.,0.,0.));
#6309=DIRECTION('ref_axis',(0.,1.,0.));
#6310=DIRECTION('',(0.,1.,0.));
#6311=DIRECTION('',(0.,1.,0.));
#6312=DIRECTION('',(0.,0.,1.));
#6313=DIRECTION('center_axis',(0.,-1.,0.));
#6314=DIRECTION('ref_axis',(1.,0.,0.));
#6315=DIRECTION('',(1.,0.,0.));
#6316=DIRECTION('',(1.,0.,0.));
#6317=DIRECTION('',(0.,0.,1.));
#6318=DIRECTION('center_axis',(-1.,0.,0.));
#6319=DIRECTION('ref_axis',(0.,-1.,0.));
#6320=DIRECTION('',(0.,-1.,0.));
#6321=DIRECTION('',(0.,-1.,0.));
#6322=DIRECTION('center_axis',(0.,0.,1.));
#6323=DIRECTION('ref_axis',(1.,0.,0.));
#6324=DIRECTION('center_axis',(0.,0.,1.));
#6325=DIRECTION('ref_axis',(1.,0.,0.));
#6326=DIRECTION('axis',(0.,0.,1.));
#6327=DIRECTION('refdir',(1.,0.,0.));
#6328=DIRECTION('center_axis',(0.866025403784439,0.,-0.5));
#6329=DIRECTION('ref_axis',(0.5,0.,0.866025403784439));
#6330=DIRECTION('',(-0.5,0.,-0.866025403784439));
#6331=DIRECTION('',(0.,-1.,0.));
#6332=DIRECTION('',(0.5,0.,0.866025403784439));
#6333=DIRECTION('',(0.,-1.,0.));
#6334=DIRECTION('center_axis',(1.20185167898973E-16,0.,-1.));
#6335=DIRECTION('ref_axis',(1.,0.,1.20185167898973E-16));
#6336=DIRECTION('',(-1.,0.,-1.20185167898973E-16));
#6337=DIRECTION('',(0.,-1.,0.));
#6338=DIRECTION('',(1.,0.,1.20185167898973E-16));
#6339=DIRECTION('center_axis',(-0.866025403784439,0.,-0.5));
#6340=DIRECTION('ref_axis',(0.5,0.,-0.866025403784439));
#6341=DIRECTION('',(-0.5,0.,0.866025403784439));
#6342=DIRECTION('',(0.,-1.,0.));
#6343=DIRECTION('',(0.5,0.,-0.866025403784439));
#6344=DIRECTION('center_axis',(-0.866025403784439,0.,0.5));
#6345=DIRECTION('ref_axis',(-0.5,0.,-0.866025403784439));
#6346=DIRECTION('',(0.5,0.,0.866025403784439));
#6347=DIRECTION('',(0.,-1.,0.));
#6348=DIRECTION('',(-0.5,0.,-0.866025403784439));
#6349=DIRECTION('center_axis',(-2.40370335797945E-16,0.,1.));
#6350=DIRECTION('ref_axis',(-1.,0.,-2.40370335797945E-16));
#6351=DIRECTION('',(1.,0.,2.40370335797945E-16));
#6352=DIRECTION('',(0.,-1.,0.));
#6353=DIRECTION('',(-1.,0.,-2.40370335797945E-16));
#6354=DIRECTION('center_axis',(0.866025403784439,0.,0.5));
#6355=DIRECTION('ref_axis',(-0.5,0.,0.866025403784439));
#6356=DIRECTION('',(0.5,0.,-0.866025403784439));
#6357=DIRECTION('',(-0.5,0.,0.866025403784439));
#6358=DIRECTION('center_axis',(0.,1.,0.));
#6359=DIRECTION('ref_axis',(1.,0.,0.));
#6360=DIRECTION('center_axis',(0.,-1.,0.));
#6361=DIRECTION('ref_axis',(0.,0.,-1.));
#6362=DIRECTION('center_axis',(0.,1.,0.));
#6363=DIRECTION('ref_axis',(1.,0.,0.));
#6364=DIRECTION('center_axis',(0.,1.,0.));
#6365=DIRECTION('ref_axis',(1.,0.,0.));
#6366=DIRECTION('center_axis',(0.,1.,0.));
#6367=DIRECTION('ref_axis',(0.,0.,1.));
#6368=DIRECTION('center_axis',(0.,-1.,0.));
#6369=DIRECTION('ref_axis',(1.,0.,0.));
#6370=DIRECTION('center_axis',(0.,-1.,0.));
#6371=DIRECTION('ref_axis',(1.,0.,0.));
#6372=DIRECTION('center_axis',(0.,-1.,0.));
#6373=DIRECTION('ref_axis',(1.,0.,0.));
#6374=DIRECTION('',(0.707106781186548,0.707106781186547,8.65956056235493E-17));
#6375=DIRECTION('center_axis',(0.,-1.,0.));
#6376=DIRECTION('ref_axis',(1.,0.,0.));
#6377=DIRECTION('center_axis',(0.,-1.,0.));
#6378=DIRECTION('ref_axis',(1.,0.,0.));
#6379=DIRECTION('',(0.,1.,0.));
#6380=DIRECTION('center_axis',(0.,1.,0.));
#6381=DIRECTION('ref_axis',(1.,0.,0.));
#6382=DIRECTION('center_axis',(0.,-1.,0.));
#6383=DIRECTION('ref_axis',(1.,0.,0.));
#6384=DIRECTION('',(-0.707106781186547,0.707106781186548,-8.65956056235493E-17));
#6385=DIRECTION('center_axis',(0.,-1.,0.));
#6386=DIRECTION('ref_axis',(0.,0.,-1.));
#6387=DIRECTION('center_axis',(0.,-1.,0.));
#6388=DIRECTION('ref_axis',(1.,0.,0.));
#6389=DIRECTION('center_axis',(0.,1.,0.));
#6390=DIRECTION('ref_axis',(1.,0.,0.));
#6391=DIRECTION('center_axis',(0.,1.,0.));
#6392=DIRECTION('ref_axis',(1.,0.,0.));
#6393=DIRECTION('',(-0.447213595499958,0.894427190999916,-5.47678698264203E-17));
#6394=DIRECTION('center_axis',(0.,-1.,0.));
#6395=DIRECTION('ref_axis',(1.,0.,0.));
#6396=DIRECTION('',(0.,1.,0.));
#6397=DIRECTION('axis',(0.,0.,1.));
#6398=DIRECTION('refdir',(1.,0.,0.));
#6399=DIRECTION('axis',(0.,0.,1.));
#6400=DIRECTION('refdir',(1.,0.,0.));
#6401=DIRECTION('center_axis',(0.,1.,0.));
#6402=DIRECTION('ref_axis',(1.,0.,0.));
#6403=DIRECTION('center_axis',(0.,1.,0.));
#6404=DIRECTION('ref_axis',(1.,0.,0.));
#6405=DIRECTION('',(0.,1.,0.));
#6406=DIRECTION('center_axis',(0.,-1.,0.));
#6407=DIRECTION('ref_axis',(1.,0.,0.));
#6408=DIRECTION('center_axis',(0.,1.,0.));
#6409=DIRECTION('ref_axis',(1.,0.,0.));
#6410=DIRECTION('center_axis',(0.,1.,0.));
#6411=DIRECTION('ref_axis',(1.,0.,0.));
#6412=DIRECTION('center_axis',(0.,1.,0.));
#6413=DIRECTION('ref_axis',(1.,0.,0.));
#6414=DIRECTION('',(0.5,0.,-0.866025403784439));
#6415=DIRECTION('',(-0.5,0.,-0.866025403784439));
#6416=DIRECTION('',(-1.,0.,-1.60246890531964E-16));
#6417=DIRECTION('',(-0.5,0.,0.866025403784439));
#6418=DIRECTION('',(0.5,0.,0.866025403784439));
#6419=DIRECTION('',(1.,0.,1.60246890531964E-16));
#6420=DIRECTION('center_axis',(0.,-1.,0.));
#6421=DIRECTION('ref_axis',(1.,0.,0.));
#6422=DIRECTION('center_axis',(0.,1.,0.));
#6423=DIRECTION('ref_axis',(1.,0.,0.));
#6424=DIRECTION('',(0.5,0.,-0.866025403784439));
#6425=DIRECTION('',(1.,0.,1.60246890531964E-16));
#6426=DIRECTION('',(0.5,0.,0.866025403784439));
#6427=DIRECTION('',(-0.5,0.,0.866025403784439));
#6428=DIRECTION('',(-1.,0.,-1.60246890531964E-16));
#6429=DIRECTION('',(-0.5,0.,-0.866025403784439));
#6430=DIRECTION('center_axis',(0.,-1.,0.));
#6431=DIRECTION('ref_axis',(1.,0.,0.));
#6432=DIRECTION('center_axis',(-1.60246890531964E-16,0.,1.));
#6433=DIRECTION('ref_axis',(1.,0.,1.60246890531964E-16));
#6434=DIRECTION('',(0.,1.,0.));
#6435=DIRECTION('',(0.,1.,0.));
#6436=DIRECTION('center_axis',(-0.866025403784439,0.,0.5));
#6437=DIRECTION('ref_axis',(0.5,0.,0.866025403784439));
#6438=DIRECTION('',(0.,1.,0.));
#6439=DIRECTION('center_axis',(-0.866025403784439,0.,-0.5));
#6440=DIRECTION('ref_axis',(-0.5,0.,0.866025403784439));
#6441=DIRECTION('',(0.,1.,0.));
#6442=DIRECTION('center_axis',(1.60246890531964E-16,0.,-1.));
#6443=DIRECTION('ref_axis',(-1.,0.,-1.60246890531964E-16));
#6444=DIRECTION('',(0.,1.,0.));
#6445=DIRECTION('center_axis',(0.866025403784439,0.,-0.5));
#6446=DIRECTION('ref_axis',(-0.5,0.,-0.866025403784439));
#6447=DIRECTION('',(0.,1.,0.));
#6448=DIRECTION('center_axis',(0.866025403784439,0.,0.5));
#6449=DIRECTION('ref_axis',(0.5,0.,-0.866025403784439));
#6450=DIRECTION('center_axis',(0.,1.,0.));
#6451=DIRECTION('ref_axis',(0.,0.,1.));
#6452=DIRECTION('center_axis',(0.,-1.,0.));
#6453=DIRECTION('ref_axis',(1.,0.,0.));
#6454=DIRECTION('center_axis',(0.,-1.,0.));
#6455=DIRECTION('ref_axis',(1.,0.,0.));
#6456=DIRECTION('',(0.,1.,0.));
#6457=DIRECTION('center_axis',(0.,-1.,0.));
#6458=DIRECTION('ref_axis',(1.,0.,0.));
#6459=DIRECTION('center_axis',(0.,1.,0.));
#6460=DIRECTION('ref_axis',(0.,0.,1.));
#6461=DIRECTION('center_axis',(0.,-1.,0.));
#6462=DIRECTION('ref_axis',(1.,0.,0.));
#6463=DIRECTION('center_axis',(0.,-1.,0.));
#6464=DIRECTION('ref_axis',(1.,0.,0.));
#6465=DIRECTION('',(0.,1.,0.));
#6466=DIRECTION('center_axis',(0.,-1.,0.));
#6467=DIRECTION('ref_axis',(1.,0.,0.));
#6468=DIRECTION('center_axis',(0.,-1.,0.));
#6469=DIRECTION('ref_axis',(1.,0.,0.));
#6470=DIRECTION('',(0.,1.,0.));
#6471=DIRECTION('center_axis',(0.,-1.,0.));
#6472=DIRECTION('ref_axis',(0.,0.,-1.));
#6473=DIRECTION('center_axis',(0.,-1.,0.));
#6474=DIRECTION('ref_axis',(1.,0.,0.));
#6475=DIRECTION('center_axis',(0.,-1.,0.));
#6476=DIRECTION('ref_axis',(1.,0.,0.));
#6477=DIRECTION('',(0.,1.,0.));
#6478=DIRECTION('axis',(0.,0.,1.));
#6479=DIRECTION('refdir',(1.,0.,0.));
#6480=DIRECTION('center_axis',(0.,1.,0.));
#6481=DIRECTION('ref_axis',(0.,0.,1.));
#6482=DIRECTION('center_axis',(0.,-1.,0.));
#6483=DIRECTION('ref_axis',(1.,0.,0.));
#6484=DIRECTION('center_axis',(0.,-1.,0.));
#6485=DIRECTION('ref_axis',(1.,0.,0.));
#6486=DIRECTION('center_axis',(0.,-1.,0.));
#6487=DIRECTION('ref_axis',(1.,0.,0.));
#6488=DIRECTION('center_axis',(0.,-1.,0.));
#6489=DIRECTION('ref_axis',(1.,0.,0.));
#6490=DIRECTION('',(0.,1.,0.));
#6491=DIRECTION('center_axis',(0.,-1.,0.));
#6492=DIRECTION('ref_axis',(0.,0.,-1.));
#6493=DIRECTION('center_axis',(0.,-1.,0.));
#6494=DIRECTION('ref_axis',(1.,0.,0.));
#6495=DIRECTION('center_axis',(0.,-1.,0.));
#6496=DIRECTION('ref_axis',(1.,0.,0.));
#6497=DIRECTION('center_axis',(0.,-1.,0.));
#6498=DIRECTION('ref_axis',(1.,0.,0.));
#6499=DIRECTION('',(0.,1.,0.));
#6500=DIRECTION('center_axis',(0.,-1.,0.));
#6501=DIRECTION('ref_axis',(0.,0.,-1.));
#6502=DIRECTION('center_axis',(0.,-1.,0.));
#6503=DIRECTION('ref_axis',(1.,0.,0.));
#6504=DIRECTION('center_axis',(0.,-1.,0.));
#6505=DIRECTION('ref_axis',(1.,0.,0.));
#6506=DIRECTION('',(0.,1.,0.));
#6507=DIRECTION('',(0.,0.,1.));
#6508=DIRECTION('',(1.,0.,0.));
#6509=DIRECTION('',(0.,0.,1.));
#6510=DIRECTION('',(1.,0.,0.));
#6511=DIRECTION('axis',(0.,0.,1.));
#6512=DIRECTION('refdir',(1.,0.,0.));
#6513=DIRECTION('center_axis',(0.,1.,0.));
#6514=DIRECTION('ref_axis',(1.,0.,0.));
#6515=DIRECTION('',(-0.5,0.,0.866025403784439));
#6516=DIRECTION('',(-1.,0.,-3.29650746237182E-16));
#6517=DIRECTION('',(-0.5,0.,-0.866025403784439));
#6518=DIRECTION('',(0.5,0.,-0.866025403784438));
#6519=DIRECTION('',(1.,0.,0.));
#6520=DIRECTION('',(0.5,0.,0.866025403784439));
#6521=DIRECTION('center_axis',(0.,-1.,0.));
#6522=DIRECTION('ref_axis',(1.,0.,0.));
#6523=DIRECTION('center_axis',(0.,1.,0.));
#6524=DIRECTION('ref_axis',(1.,0.,0.));
#6525=DIRECTION('',(0.5,0.,-0.866025403784439));
#6526=DIRECTION('',(-0.5,0.,-0.866025403784439));
#6527=DIRECTION('',(-1.,0.,0.));
#6528=DIRECTION('',(-0.5,0.,0.866025403784438));
#6529=DIRECTION('',(0.5,0.,0.866025403784439));
#6530=DIRECTION('',(1.,0.,3.29650746237182E-16));
#6531=DIRECTION('center_axis',(0.,1.,0.));
#6532=DIRECTION('ref_axis',(1.,0.,0.));
#6533=DIRECTION('center_axis',(-3.29650746237182E-16,0.,1.));
#6534=DIRECTION('ref_axis',(1.,0.,3.29650746237182E-16));
#6535=DIRECTION('',(0.,-1.,0.));
#6536=DIRECTION('',(0.,1.,0.));
#6537=DIRECTION('center_axis',(-0.866025403784439,0.,0.5));
#6538=DIRECTION('ref_axis',(0.5,0.,0.866025403784439));
#6539=DIRECTION('',(0.,1.,0.));
#6540=DIRECTION('center_axis',(-0.866025403784439,0.,-0.5));
#6541=DIRECTION('ref_axis',(-0.5,0.,0.866025403784439));
#6542=DIRECTION('',(0.,1.,0.));
#6543=DIRECTION('center_axis',(0.,0.,-1.));
#6544=DIRECTION('ref_axis',(-1.,0.,0.));
#6545=DIRECTION('',(0.,1.,0.));
#6546=DIRECTION('center_axis',(0.866025403784439,0.,-0.5));
#6547=DIRECTION('ref_axis',(-0.5,0.,-0.866025403784439));
#6548=DIRECTION('',(0.,1.,0.));
#6549=DIRECTION('center_axis',(0.866025403784439,0.,0.5));
#6550=DIRECTION('ref_axis',(0.5,0.,-0.866025403784439));
#6551=DIRECTION('center_axis',(0.,-1.,0.));
#6552=DIRECTION('ref_axis',(1.,0.,0.));
#6553=DIRECTION('',(0.,1.,0.));
#6554=DIRECTION('center_axis',(0.,-1.,0.));
#6555=DIRECTION('ref_axis',(1.,0.,0.));
#6556=DIRECTION('center_axis',(0.,1.,0.));
#6557=DIRECTION('ref_axis',(0.,0.,1.));
#6558=DIRECTION('center_axis',(0.,-1.,0.));
#6559=DIRECTION('ref_axis',(1.,0.,0.));
#6560=DIRECTION('center_axis',(0.,-1.,0.));
#6561=DIRECTION('ref_axis',(1.,0.,0.));
#6562=DIRECTION('center_axis',(0.,-1.,0.));
#6563=DIRECTION('ref_axis',(1.,0.,0.));
#6564=DIRECTION('',(0.707106781186547,0.707106781186548,8.65956056235493E-17));
#6565=DIRECTION('center_axis',(0.,-1.,0.));
#6566=DIRECTION('ref_axis',(1.,0.,0.));
#6567=DIRECTION('center_axis',(0.,-1.,0.));
#6568=DIRECTION('ref_axis',(1.,0.,0.));
#6569=DIRECTION('',(0.,1.,0.));
#6570=DIRECTION('center_axis',(0.,1.,0.));
#6571=DIRECTION('ref_axis',(1.,0.,0.));
#6572=DIRECTION('center_axis',(0.,-1.,0.));
#6573=DIRECTION('ref_axis',(1.,0.,0.));
#6574=DIRECTION('',(-0.707106781186547,0.707106781186548,-8.65956056235493E-17));
#6575=DIRECTION('center_axis',(0.,-1.,0.));
#6576=DIRECTION('ref_axis',(0.,0.,-1.));
#6577=DIRECTION('center_axis',(0.,-1.,0.));
#6578=DIRECTION('ref_axis',(1.,0.,0.));
#6579=DIRECTION('center_axis',(0.,-1.,0.));
#6580=DIRECTION('ref_axis',(1.,0.,0.));
#6581=DIRECTION('',(0.,1.,0.));
#6582=DIRECTION('axis',(0.,0.,1.));
#6583=DIRECTION('refdir',(1.,0.,0.));
#6584=DIRECTION('center_axis',(0.,1.,0.));
#6585=DIRECTION('ref_axis',(0.,0.,1.));
#6586=DIRECTION('center_axis',(0.,-1.,0.));
#6587=DIRECTION('ref_axis',(1.,0.,0.));
#6588=DIRECTION('center_axis',(0.,-1.,0.));
#6589=DIRECTION('ref_axis',(1.,0.,0.));
#6590=DIRECTION('center_axis',(0.,-1.,0.));
#6591=DIRECTION('ref_axis',(1.,0.,0.));
#6592=DIRECTION('',(0.707106781186547,0.707106781186548,8.65956056235493E-17));
#6593=DIRECTION('center_axis',(0.,-1.,0.));
#6594=DIRECTION('ref_axis',(1.,0.,0.));
#6595=DIRECTION('center_axis',(0.,-1.,0.));
#6596=DIRECTION('ref_axis',(1.,0.,0.));
#6597=DIRECTION('',(0.,1.,0.));
#6598=DIRECTION('center_axis',(0.,1.,0.));
#6599=DIRECTION('ref_axis',(1.,0.,0.));
#6600=DIRECTION('center_axis',(0.,-1.,0.));
#6601=DIRECTION('ref_axis',(1.,0.,0.));
#6602=DIRECTION('',(-0.707106781186547,0.707106781186548,-8.65956056235493E-17));
#6603=DIRECTION('center_axis',(0.,-1.,0.));
#6604=DIRECTION('ref_axis',(0.,0.,-1.));
#6605=DIRECTION('center_axis',(0.,-1.,0.));
#6606=DIRECTION('ref_axis',(1.,0.,0.));
#6607=DIRECTION('center_axis',(0.,1.,0.));
#6608=DIRECTION('ref_axis',(1.,0.,0.));
#6609=DIRECTION('center_axis',(0.,1.,0.));
#6610=DIRECTION('ref_axis',(1.,0.,0.));
#6611=DIRECTION('',(-0.447213595499958,0.894427190999916,-5.47678698264203E-17));
#6612=DIRECTION('center_axis',(0.,-1.,0.));
#6613=DIRECTION('ref_axis',(1.,0.,0.));
#6614=DIRECTION('center_axis',(0.,1.,0.));
#6615=DIRECTION('ref_axis',(1.,0.,0.));
#6616=DIRECTION('',(0.,1.,0.));
#6617=DIRECTION('center_axis',(0.,1.,0.));
#6618=DIRECTION('ref_axis',(1.,0.,0.));
#6619=DIRECTION('center_axis',(0.,-1.,0.));
#6620=DIRECTION('ref_axis',(1.,0.,0.));
#6621=DIRECTION('',(-0.707106781186547,0.707106781186548,-8.65956056235493E-17));
#6622=DIRECTION('center_axis',(0.,-1.,0.));
#6623=DIRECTION('ref_axis',(0.,0.,-1.));
#6624=DIRECTION('center_axis',(0.866025403784439,0.,-0.5));
#6625=DIRECTION('ref_axis',(0.5,0.,0.866025403784439));
#6626=DIRECTION('',(-0.5,0.,-0.866025403784439));
#6627=DIRECTION('',(0.,-1.,0.));
#6628=DIRECTION('',(0.5,0.,0.866025403784439));
#6629=DIRECTION('',(0.,-1.,0.));
#6630=DIRECTION('center_axis',(1.60246890531964E-16,0.,-1.));
#6631=DIRECTION('ref_axis',(1.,0.,1.60246890531964E-16));
#6632=DIRECTION('',(-1.,0.,-1.60246890531964E-16));
#6633=DIRECTION('',(0.,-1.,0.));
#6634=DIRECTION('',(1.,0.,1.60246890531964E-16));
#6635=DIRECTION('center_axis',(-0.866025403784439,0.,-0.5));
#6636=DIRECTION('ref_axis',(0.5,0.,-0.866025403784439));
#6637=DIRECTION('',(-0.5,0.,0.866025403784439));
#6638=DIRECTION('',(0.,-1.,0.));
#6639=DIRECTION('',(0.5,0.,-0.866025403784439));
#6640=DIRECTION('center_axis',(-0.866025403784439,0.,0.5));
#6641=DIRECTION('ref_axis',(-0.5,0.,-0.866025403784439));
#6642=DIRECTION('',(0.5,0.,0.866025403784439));
#6643=DIRECTION('',(0.,-1.,0.));
#6644=DIRECTION('',(-0.5,0.,-0.866025403784439));
#6645=DIRECTION('center_axis',(-1.60246890531964E-16,0.,1.));
#6646=DIRECTION('ref_axis',(-1.,0.,-1.60246890531964E-16));
#6647=DIRECTION('',(1.,0.,1.60246890531964E-16));
#6648=DIRECTION('',(0.,-1.,0.));
#6649=DIRECTION('',(-1.,0.,-1.60246890531964E-16));
#6650=DIRECTION('center_axis',(0.866025403784439,0.,0.5));
#6651=DIRECTION('ref_axis',(-0.5,0.,0.866025403784439));
#6652=DIRECTION('',(0.5,0.,-0.866025403784439));
#6653=DIRECTION('',(-0.5,0.,0.866025403784439));
#6654=DIRECTION('center_axis',(0.,1.,0.));
#6655=DIRECTION('ref_axis',(1.,0.,0.));
#6656=DIRECTION('center_axis',(0.,-1.,0.));
#6657=DIRECTION('ref_axis',(0.,0.,-1.));
#6658=DIRECTION('axis',(0.,0.,1.));
#6659=DIRECTION('refdir',(1.,0.,0.));
#6660=DIRECTION('center_axis',(0.866025403784439,0.,-0.5));
#6661=DIRECTION('ref_axis',(0.5,0.,0.866025403784439));
#6662=DIRECTION('',(-0.5,0.,-0.866025403784439));
#6663=DIRECTION('',(0.,-1.,0.));
#6664=DIRECTION('',(0.5,0.,0.866025403784439));
#6665=DIRECTION('',(0.,-1.,0.));
#6666=DIRECTION('center_axis',(1.60246890531964E-16,0.,-1.));
#6667=DIRECTION('ref_axis',(1.,0.,1.60246890531964E-16));
#6668=DIRECTION('',(-1.,0.,-1.60246890531964E-16));
#6669=DIRECTION('',(0.,-1.,0.));
#6670=DIRECTION('',(1.,0.,1.60246890531964E-16));
#6671=DIRECTION('center_axis',(-0.866025403784439,0.,-0.5));
#6672=DIRECTION('ref_axis',(0.5,0.,-0.866025403784439));
#6673=DIRECTION('',(-0.5,0.,0.866025403784439));
#6674=DIRECTION('',(0.,-1.,0.));
#6675=DIRECTION('',(0.5,0.,-0.866025403784439));
#6676=DIRECTION('center_axis',(-0.866025403784439,0.,0.5));
#6677=DIRECTION('ref_axis',(-0.5,0.,-0.866025403784439));
#6678=DIRECTION('',(0.5,0.,0.866025403784439));
#6679=DIRECTION('',(0.,-1.,0.));
#6680=DIRECTION('',(-0.5,0.,-0.866025403784439));
#6681=DIRECTION('center_axis',(-1.60246890531964E-16,0.,1.));
#6682=DIRECTION('ref_axis',(-1.,0.,-1.60246890531964E-16));
#6683=DIRECTION('',(1.,0.,1.60246890531964E-16));
#6684=DIRECTION('',(0.,-1.,0.));
#6685=DIRECTION('',(-1.,0.,-1.60246890531964E-16));
#6686=DIRECTION('center_axis',(0.866025403784439,0.,0.5));
#6687=DIRECTION('ref_axis',(-0.5,0.,0.866025403784439));
#6688=DIRECTION('',(0.5,0.,-0.866025403784439));
#6689=DIRECTION('',(-0.5,0.,0.866025403784439));
#6690=DIRECTION('center_axis',(0.,1.,0.));
#6691=DIRECTION('ref_axis',(1.,0.,0.));
#6692=DIRECTION('center_axis',(0.,-1.,0.));
#6693=DIRECTION('ref_axis',(0.,0.,-1.));
#6694=DIRECTION('center_axis',(0.,1.,0.));
#6695=DIRECTION('ref_axis',(1.,0.,0.));
#6696=DIRECTION('center_axis',(0.,1.,0.));
#6697=DIRECTION('ref_axis',(1.,0.,0.));
#6698=DIRECTION('center_axis',(0.,1.,0.));
#6699=DIRECTION('ref_axis',(0.,0.,1.));
#6700=DIRECTION('center_axis',(0.,-1.,0.));
#6701=DIRECTION('ref_axis',(1.,0.,0.));
#6702=DIRECTION('center_axis',(0.,-1.,0.));
#6703=DIRECTION('ref_axis',(1.,0.,0.));
#6704=DIRECTION('center_axis',(0.,-1.,0.));
#6705=DIRECTION('ref_axis',(1.,0.,0.));
#6706=DIRECTION('',(0.707106781186547,0.707106781186548,8.65956056235493E-17));
#6707=DIRECTION('center_axis',(0.,-1.,0.));
#6708=DIRECTION('ref_axis',(1.,0.,0.));
#6709=DIRECTION('center_axis',(0.,-1.,0.));
#6710=DIRECTION('ref_axis',(1.,0.,0.));
#6711=DIRECTION('',(0.,1.,0.));
#6712=DIRECTION('center_axis',(0.,1.,0.));
#6713=DIRECTION('ref_axis',(1.,0.,0.));
#6714=DIRECTION('center_axis',(0.,-1.,0.));
#6715=DIRECTION('ref_axis',(1.,0.,0.));
#6716=DIRECTION('',(-0.707106781186547,0.707106781186548,-8.65956056235493E-17));
#6717=DIRECTION('center_axis',(0.,-1.,0.));
#6718=DIRECTION('ref_axis',(0.,0.,-1.));
#6719=DIRECTION('center_axis',(0.,-1.,0.));
#6720=DIRECTION('ref_axis',(1.,0.,0.));
#6721=DIRECTION('center_axis',(0.,1.,0.));
#6722=DIRECTION('ref_axis',(1.,0.,0.));
#6723=DIRECTION('center_axis',(0.,1.,0.));
#6724=DIRECTION('ref_axis',(1.,0.,0.));
#6725=DIRECTION('',(-0.447213595499958,0.894427190999916,-5.47678698264203E-17));
#6726=DIRECTION('center_axis',(0.,-1.,0.));
#6727=DIRECTION('ref_axis',(1.,0.,0.));
#6728=DIRECTION('',(0.,1.,0.));
#6729=DIRECTION('',(0.,0.,1.));
#6730=DIRECTION('',(1.,0.,0.));
#6731=DIRECTION('',(0.,0.,1.));
#6732=DIRECTION('',(1.,0.,0.));
#6733=DIRECTION('',(0.,0.,1.));
#6734=DIRECTION('',(1.,0.,0.));
#6735=DIRECTION('',(0.,0.,1.));
#6736=DIRECTION('',(1.,0.,0.));
#6737=DIRECTION('',(0.,0.,1.));
#6738=DIRECTION('',(1.,0.,0.));
#6739=DIRECTION('',(0.,0.,1.));
#6740=DIRECTION('',(1.,0.,0.));
#6741=DIRECTION('',(0.,0.,1.));
#6742=DIRECTION('',(1.,0.,0.));
#6743=DIRECTION('',(0.,0.,1.));
#6744=DIRECTION('',(1.,0.,0.));
#6745=DIRECTION('',(0.,0.,1.));
#6746=DIRECTION('',(1.,0.,0.));
#6747=DIRECTION('',(0.,0.,1.));
#6748=DIRECTION('',(1.,0.,0.));
#6749=DIRECTION('',(0.,0.,1.));
#6750=DIRECTION('',(1.,0.,0.));
#6751=DIRECTION('',(0.,0.,1.));
#6752=DIRECTION('',(1.,0.,0.));
#6753=DIRECTION('',(0.,0.,1.));
#6754=DIRECTION('',(1.,0.,0.));
#6755=DIRECTION('',(0.,0.,1.));
#6756=DIRECTION('',(1.,0.,0.));
#6757=DIRECTION('',(0.,0.,1.));
#6758=DIRECTION('',(1.,0.,0.));
#6759=DIRECTION('',(0.,0.,1.));
#6760=DIRECTION('',(1.,0.,0.));
#6761=DIRECTION('',(0.,-1.,2.22044604925031E-16));
#6762=DIRECTION('',(1.,0.,0.));
#6763=DIRECTION('',(0.,-1.,2.22044604925031E-16));
#6764=DIRECTION('',(1.,0.,0.));
#6765=DIRECTION('',(0.,1.,2.22044604925031E-16));
#6766=DIRECTION('',(1.,0.,0.));
#6767=DIRECTION('',(0.,1.,2.22044604925031E-16));
#6768=DIRECTION('',(1.,0.,0.));
#6769=DIRECTION('',(0.,-1.,2.22044604925031E-16));
#6770=DIRECTION('',(1.,0.,0.));
#6771=DIRECTION('',(0.,-1.,2.22044604925031E-16));
#6772=DIRECTION('',(1.,0.,0.));
#6773=DIRECTION('',(0.,1.,2.22044604925031E-16));
#6774=DIRECTION('',(1.,0.,0.));
#6775=DIRECTION('',(0.,1.,2.22044604925031E-16));
#6776=DIRECTION('',(1.,0.,0.));
#6777=DIRECTION('',(0.,-1.,2.22044604925031E-16));
#6778=DIRECTION('',(1.,0.,0.));
#6779=DIRECTION('',(0.,-1.,2.22044604925031E-16));
#6780=DIRECTION('',(1.,0.,0.));
#6781=DIRECTION('',(0.,-1.,2.22044604925031E-16));
#6782=DIRECTION('',(1.,0.,0.));
#6783=DIRECTION('',(0.,-1.,2.22044604925031E-16));
#6784=DIRECTION('',(1.,0.,0.));
#6785=DIRECTION('',(0.,0.,1.));
#6786=DIRECTION('',(2.22044604925031E-16,-1.,0.));
#6787=DIRECTION('',(0.,1.,2.22044604925031E-16));
#6788=DIRECTION('',(1.,0.,0.));
#6789=DIRECTION('',(0.,1.,2.22044604925031E-16));
#6790=DIRECTION('',(1.,0.,0.));
#6791=DIRECTION('',(0.,1.,2.22044604925031E-16));
#6792=DIRECTION('',(1.,0.,0.));
#6793=DIRECTION('',(0.,1.,2.22044604925031E-16));
#6794=DIRECTION('',(1.,0.,0.));
#6795=DIRECTION('',(0.,1.,2.22044604925031E-16));
#6796=DIRECTION('',(1.,0.,0.));
#6797=DIRECTION('',(0.,1.,2.22044604925031E-16));
#6798=DIRECTION('',(1.,0.,0.));
#6799=DIRECTION('',(0.,0.,1.));
#6800=DIRECTION('',(-1.,1.22464679914735E-16,0.));
#6801=DIRECTION('',(0.,0.,1.));
#6802=DIRECTION('',(-1.,1.22464679914735E-16,0.));
#6803=CARTESIAN_POINT('',(0.,0.,0.));
#6804=CARTESIAN_POINT('',(0.,0.,0.));
#6805=CARTESIAN_POINT('Origin',(5.,-1.8,-0.2));
#6806=CARTESIAN_POINT('',(4.5,-1.8,-0.2));
#6807=CARTESIAN_POINT('Origin',(5.,-1.8,-0.2));
#6808=CARTESIAN_POINT('',(4.5,-1.8,0.4));
#6809=CARTESIAN_POINT('',(4.5,-1.8,-0.2));
#6810=CARTESIAN_POINT('Origin',(5.,-1.8,0.4));
#6811=CARTESIAN_POINT('Origin',(5.,-1.8,-0.2));
#6812=CARTESIAN_POINT('Origin',(-5.,1.8,-0.2));
#6813=CARTESIAN_POINT('',(-5.5,1.8,-0.2));
#6814=CARTESIAN_POINT('Origin',(-5.,1.8,-0.2));
#6815=CARTESIAN_POINT('',(-5.5,1.8,0.4));
#6816=CARTESIAN_POINT('',(-5.5,1.8,-0.2));
#6817=CARTESIAN_POINT('Origin',(-5.,1.8,0.4));
#6818=CARTESIAN_POINT('Origin',(-5.,1.8,-0.2));
#6819=CARTESIAN_POINT('Origin',(-5.,-1.8,-0.2));
#6820=CARTESIAN_POINT('',(-5.5,-1.8,-0.2));
#6821=CARTESIAN_POINT('Origin',(-5.,-1.8,-0.2));
#6822=CARTESIAN_POINT('',(-5.5,-1.8,0.4));
#6823=CARTESIAN_POINT('',(-5.5,-1.8,-0.2));
#6824=CARTESIAN_POINT('Origin',(-5.,-1.8,0.4));
#6825=CARTESIAN_POINT('Origin',(-5.,-1.8,-0.2));
#6826=CARTESIAN_POINT('Origin',(5.,1.8,-0.2));
#6827=CARTESIAN_POINT('',(4.5,1.8,-0.2));
#6828=CARTESIAN_POINT('Origin',(5.,1.8,-0.2));
#6829=CARTESIAN_POINT('',(4.5,1.8,0.4));
#6830=CARTESIAN_POINT('',(4.5,1.8,-0.2));
#6831=CARTESIAN_POINT('Origin',(5.,1.8,0.4));
#6832=CARTESIAN_POINT('Origin',(5.,1.8,-0.2));
#6833=CARTESIAN_POINT('Origin',(5.,-2.8,-0.5));
#6834=CARTESIAN_POINT('',(4.79,-2.8,-0.4));
#6835=CARTESIAN_POINT('Origin',(5.,-2.8,-0.4));
#6836=CARTESIAN_POINT('',(4.79,-2.8,0.4));
#6837=CARTESIAN_POINT('',(4.79,-2.8,-0.5));
#6838=CARTESIAN_POINT('Origin',(5.,-2.8,0.4));
#6839=CARTESIAN_POINT('Origin',(-5.,2.8,-0.5));
#6840=CARTESIAN_POINT('',(-5.21,2.8,-0.4));
#6841=CARTESIAN_POINT('Origin',(-5.,2.8,-0.4));
#6842=CARTESIAN_POINT('',(-5.21,2.8,0.4));
#6843=CARTESIAN_POINT('',(-5.21,2.8,-0.5));
#6844=CARTESIAN_POINT('Origin',(-5.,2.8,0.4));
#6845=CARTESIAN_POINT('Origin',(-5.,-2.8,-0.5));
#6846=CARTESIAN_POINT('',(-5.21,-2.8,-0.4));
#6847=CARTESIAN_POINT('Origin',(-5.,-2.8,-0.4));
#6848=CARTESIAN_POINT('',(-5.21,-2.8,0.4));
#6849=CARTESIAN_POINT('',(-5.21,-2.8,-0.5));
#6850=CARTESIAN_POINT('Origin',(-5.,-2.8,0.4));
#6851=CARTESIAN_POINT('Origin',(5.,2.8,-0.5));
#6852=CARTESIAN_POINT('',(4.79,2.8,-0.4));
#6853=CARTESIAN_POINT('Origin',(5.,2.8,-0.4));
#6854=CARTESIAN_POINT('',(4.79,2.8,0.4));
#6855=CARTESIAN_POINT('',(4.79,2.8,-0.5));
#6856=CARTESIAN_POINT('Origin',(5.,2.8,0.4));
#6857=CARTESIAN_POINT('Origin',(8.,5.,-0.4));
#6858=CARTESIAN_POINT('',(8.,5.,-0.4));
#6859=CARTESIAN_POINT('',(-8.,5.,-0.4));
#6860=CARTESIAN_POINT('',(8.,5.,-0.4));
#6861=CARTESIAN_POINT('',(-8.,5.,0.4));
#6862=CARTESIAN_POINT('',(-8.,5.,-0.4));
#6863=CARTESIAN_POINT('',(8.,5.,0.4));
#6864=CARTESIAN_POINT('',(8.,5.,0.4));
#6865=CARTESIAN_POINT('',(8.,5.,-0.4));
#6866=CARTESIAN_POINT('Origin',(8.,-5.,-0.4));
#6867=CARTESIAN_POINT('',(8.,-5.,-0.4));
#6868=CARTESIAN_POINT('',(8.,-5.,-0.4));
#6869=CARTESIAN_POINT('',(8.,-5.,0.4));
#6870=CARTESIAN_POINT('',(8.,-5.,0.4));
#6871=CARTESIAN_POINT('',(8.,-5.,-0.4));
#6872=CARTESIAN_POINT('Origin',(-8.,-5.,-0.4));
#6873=CARTESIAN_POINT('',(-8.,-5.,-0.4));
#6874=CARTESIAN_POINT('',(-8.,-5.,-0.4));
#6875=CARTESIAN_POINT('',(-8.,-5.,0.4));
#6876=CARTESIAN_POINT('',(-8.,-5.,0.4));
#6877=CARTESIAN_POINT('',(-8.,-5.,-0.4));
#6878=CARTESIAN_POINT('Origin',(-8.,5.,-0.4));
#6879=CARTESIAN_POINT('',(-8.,5.,-0.4));
#6880=CARTESIAN_POINT('',(-8.,5.,0.4));
#6881=CARTESIAN_POINT('Origin',(0.,0.,0.4));
#6882=CARTESIAN_POINT('Origin',(0.,0.,-0.4));
#6883=CARTESIAN_POINT('',(0.,0.,0.));
#6884=CARTESIAN_POINT('Origin',(-6.,5.,-0.7));
#6885=CARTESIAN_POINT('',(-6.,5.,-0.7));
#6886=CARTESIAN_POINT('',(-8.,5.,-0.7));
#6887=CARTESIAN_POINT('',(-6.,5.,-0.7));
#6888=CARTESIAN_POINT('',(-8.,5.,-0.4));
#6889=CARTESIAN_POINT('',(-8.,5.,-0.7));
#6890=CARTESIAN_POINT('',(-6.,5.,-0.4));
#6891=CARTESIAN_POINT('',(-6.,5.,-0.4));
#6892=CARTESIAN_POINT('',(-6.,5.,-0.7));
#6893=CARTESIAN_POINT('Origin',(-6.,-5.,-0.7));
#6894=CARTESIAN_POINT('',(-6.,-5.,-0.7));
#6895=CARTESIAN_POINT('',(-6.,-5.,-0.7));
#6896=CARTESIAN_POINT('',(-6.,-5.,-0.4));
#6897=CARTESIAN_POINT('',(-6.,-5.,-0.4));
#6898=CARTESIAN_POINT('',(-6.,-5.,-0.7));
#6899=CARTESIAN_POINT('Origin',(-8.,-5.,-0.7));
#6900=CARTESIAN_POINT('',(-8.,-5.,-0.7));
#6901=CARTESIAN_POINT('',(-8.,-5.,-0.7));
#6902=CARTESIAN_POINT('',(-8.,-5.,-0.4));
#6903=CARTESIAN_POINT('',(-8.,-5.,-0.4));
#6904=CARTESIAN_POINT('',(-8.,-5.,-0.7));
#6905=CARTESIAN_POINT('Origin',(-8.,5.,-0.7));
#6906=CARTESIAN_POINT('',(-8.,5.,-0.7));
#6907=CARTESIAN_POINT('',(-8.,5.,-0.4));
#6908=CARTESIAN_POINT('Origin',(-7.,0.,-0.4));
#6909=CARTESIAN_POINT('Origin',(-7.,0.,-0.7));
#6910=CARTESIAN_POINT('',(0.,0.,0.));
#6911=CARTESIAN_POINT('Origin',(8.,5.,-0.7));
#6912=CARTESIAN_POINT('',(8.,5.,-0.7));
#6913=CARTESIAN_POINT('',(6.,5.,-0.7));
#6914=CARTESIAN_POINT('',(8.,5.,-0.7));
#6915=CARTESIAN_POINT('',(6.,5.,-0.4));
#6916=CARTESIAN_POINT('',(6.,5.,-0.7));
#6917=CARTESIAN_POINT('',(8.,5.,-0.4));
#6918=CARTESIAN_POINT('',(8.,5.,-0.4));
#6919=CARTESIAN_POINT('',(8.,5.,-0.7));
#6920=CARTESIAN_POINT('Origin',(8.,-5.,-0.7));
#6921=CARTESIAN_POINT('',(8.,-5.,-0.7));
#6922=CARTESIAN_POINT('',(8.,-5.,-0.7));
#6923=CARTESIAN_POINT('',(8.,-5.,-0.4));
#6924=CARTESIAN_POINT('',(8.,-5.,-0.4));
#6925=CARTESIAN_POINT('',(8.,-5.,-0.7));
#6926=CARTESIAN_POINT('Origin',(6.,-5.,-0.7));
#6927=CARTESIAN_POINT('',(6.,-5.,-0.7));
#6928=CARTESIAN_POINT('',(6.,-5.,-0.7));
#6929=CARTESIAN_POINT('',(6.,-5.,-0.4));
#6930=CARTESIAN_POINT('',(6.,-5.,-0.4));
#6931=CARTESIAN_POINT('',(6.,-5.,-0.7));
#6932=CARTESIAN_POINT('Origin',(6.,5.,-0.7));
#6933=CARTESIAN_POINT('',(6.,5.,-0.7));
#6934=CARTESIAN_POINT('',(6.,5.,-0.4));
#6935=CARTESIAN_POINT('Origin',(7.,0.,-0.4));
#6936=CARTESIAN_POINT('Origin',(7.,0.,-0.7));
#6937=CARTESIAN_POINT('',(0.,0.,0.));
#6938=CARTESIAN_POINT('Origin',(-4.5,-1.4,0.9));
#6939=CARTESIAN_POINT('',(-4.72519681057161,-1.78959773678549,0.9));
#6940=CARTESIAN_POINT('',(-4.92952879918449,-1.53418275101939,0.9));
#6941=CARTESIAN_POINT('Origin',(-5.,-1.8,0.9));
#6942=CARTESIAN_POINT('Origin',(-4.5,-1.4,0.9));
#6943=CARTESIAN_POINT('Origin',(-4.5,-1.4,0.9));
#6944=CARTESIAN_POINT('',(-4.72519681057161,-1.78959773678549,1.4));
#6945=CARTESIAN_POINT('',(-4.72519681057161,-1.78959773678549,0.9));
#6946=CARTESIAN_POINT('',(-4.92952879918449,-1.53418275101939,1.4));
#6947=CARTESIAN_POINT('Origin',(-4.5,-1.4,1.4));
#6948=CARTESIAN_POINT('',(-4.92952879918449,-1.53418275101939,0.9));
#6949=CARTESIAN_POINT('Origin',(-4.5,1.4,0.9));
#6950=CARTESIAN_POINT('',(-4.92952879918449,1.53418275101939,0.9));
#6951=CARTESIAN_POINT('',(-4.72519681057161,1.78959773678549,0.9));
#6952=CARTESIAN_POINT('Origin',(-5.,1.8,0.9));
#6953=CARTESIAN_POINT('Origin',(-4.5,1.4,0.9));
#6954=CARTESIAN_POINT('Origin',(-4.5,1.4,0.9));
#6955=CARTESIAN_POINT('',(-4.92952879918449,1.53418275101939,1.4));
#6956=CARTESIAN_POINT('',(-4.92952879918449,1.53418275101939,0.9));
#6957=CARTESIAN_POINT('',(-4.72519681057161,1.78959773678549,1.4));
#6958=CARTESIAN_POINT('Origin',(-4.5,1.4,1.4));
#6959=CARTESIAN_POINT('',(-4.72519681057161,1.78959773678549,0.9));
#6960=CARTESIAN_POINT('Origin',(-5.,-1.8,0.3));
#6961=CARTESIAN_POINT('',(-5.275,-1.8,0.4));
#6962=CARTESIAN_POINT('Origin',(-5.,-1.8,0.4));
#6963=CARTESIAN_POINT('',(-5.275,-1.8,1.4));
#6964=CARTESIAN_POINT('',(-5.275,-1.8,0.3));
#6965=CARTESIAN_POINT('Origin',(-5.,-1.8,1.4));
#6966=CARTESIAN_POINT('Origin',(-5.,-1.8,1.4));
#6967=CARTESIAN_POINT('Origin',(-5.,1.8,0.3));
#6968=CARTESIAN_POINT('',(-5.275,1.8,0.4));
#6969=CARTESIAN_POINT('Origin',(-5.,1.8,0.4));
#6970=CARTESIAN_POINT('',(-5.275,1.8,1.4));
#6971=CARTESIAN_POINT('',(-5.275,1.8,0.3));
#6972=CARTESIAN_POINT('Origin',(-5.,1.8,1.4));
#6973=CARTESIAN_POINT('Origin',(-5.,1.8,1.4));
#6974=CARTESIAN_POINT('Origin',(-5.,2.8,0.3));
#6975=CARTESIAN_POINT('',(-5.275,2.8,0.4));
#6976=CARTESIAN_POINT('Origin',(-5.,2.8,0.4));
#6977=CARTESIAN_POINT('',(-5.275,2.8,1.4));
#6978=CARTESIAN_POINT('',(-5.275,2.8,0.3));
#6979=CARTESIAN_POINT('Origin',(-5.,2.8,1.4));
#6980=CARTESIAN_POINT('Origin',(-5.,-2.8,0.3));
#6981=CARTESIAN_POINT('',(-5.275,-2.8,0.4));
#6982=CARTESIAN_POINT('Origin',(-5.,-2.8,0.4));
#6983=CARTESIAN_POINT('',(-5.275,-2.8,1.4));
#6984=CARTESIAN_POINT('',(-5.275,-2.8,0.3));
#6985=CARTESIAN_POINT('Origin',(-5.,-2.8,1.4));
#6986=CARTESIAN_POINT('Origin',(-4.,3.6,0.4));
#6987=CARTESIAN_POINT('',(-4.,3.6,0.4));
#6988=CARTESIAN_POINT('',(-6.,3.6,0.4));
#6989=CARTESIAN_POINT('',(-4.,3.6,0.4));
#6990=CARTESIAN_POINT('',(-6.,3.6,1.4));
#6991=CARTESIAN_POINT('',(-6.,3.6,0.4));
#6992=CARTESIAN_POINT('',(-4.,3.6,1.4));
#6993=CARTESIAN_POINT('',(-4.,3.6,1.4));
#6994=CARTESIAN_POINT('',(-4.,3.6,0.4));
#6995=CARTESIAN_POINT('Origin',(-4.,-3.6,0.4));
#6996=CARTESIAN_POINT('',(-4.,-3.6,0.4));
#6997=CARTESIAN_POINT('',(-4.,-3.6,0.4));
#6998=CARTESIAN_POINT('',(-4.,-3.6,1.4));
#6999=CARTESIAN_POINT('',(-4.,-3.6,1.4));
#7000=CARTESIAN_POINT('',(-4.,-3.6,0.4));
#7001=CARTESIAN_POINT('Origin',(-6.,-3.6,0.4));
#7002=CARTESIAN_POINT('',(-6.,-3.6,0.4));
#7003=CARTESIAN_POINT('',(-6.,-3.6,0.4));
#7004=CARTESIAN_POINT('',(-6.,-3.6,1.4));
#7005=CARTESIAN_POINT('',(-6.,-3.6,1.4));
#7006=CARTESIAN_POINT('',(-6.,-3.6,0.4));
#7007=CARTESIAN_POINT('Origin',(-6.,3.6,0.4));
#7008=CARTESIAN_POINT('',(-6.,3.6,0.4));
#7009=CARTESIAN_POINT('',(-6.,3.6,1.4));
#7010=CARTESIAN_POINT('Origin',(-5.,0.,1.4));
#7011=CARTESIAN_POINT('Origin',(-5.,0.,0.4));
#7012=CARTESIAN_POINT('',(0.,0.,0.));
#7013=CARTESIAN_POINT('Origin',(4.5,-1.4,0.9));
#7014=CARTESIAN_POINT('',(4.92952879918449,-1.53418275101939,0.9));
#7015=CARTESIAN_POINT('',(4.72519681057161,-1.78959773678549,0.9));
#7016=CARTESIAN_POINT('Origin',(5.,-1.8,0.9));
#7017=CARTESIAN_POINT('Origin',(4.5,-1.4,0.9));
#7018=CARTESIAN_POINT('Origin',(4.5,-1.4,0.9));
#7019=CARTESIAN_POINT('',(4.92952879918449,-1.53418275101939,1.4));
#7020=CARTESIAN_POINT('',(4.92952879918449,-1.53418275101939,0.9));
#7021=CARTESIAN_POINT('',(4.72519681057161,-1.78959773678549,1.4));
#7022=CARTESIAN_POINT('Origin',(4.5,-1.4,1.4));
#7023=CARTESIAN_POINT('',(4.72519681057161,-1.78959773678549,0.9));
#7024=CARTESIAN_POINT('Origin',(4.5,1.4,0.9));
#7025=CARTESIAN_POINT('',(4.72519681057161,1.78959773678549,0.9));
#7026=CARTESIAN_POINT('',(4.92952879918449,1.53418275101939,0.9));
#7027=CARTESIAN_POINT('Origin',(5.,1.8,0.9));
#7028=CARTESIAN_POINT('Origin',(4.5,1.4,0.9));
#7029=CARTESIAN_POINT('Origin',(4.5,1.4,0.9));
#7030=CARTESIAN_POINT('',(4.72519681057161,1.78959773678549,1.4));
#7031=CARTESIAN_POINT('',(4.72519681057161,1.78959773678549,0.9));
#7032=CARTESIAN_POINT('',(4.92952879918449,1.53418275101939,1.4));
#7033=CARTESIAN_POINT('Origin',(4.5,1.4,1.4));
#7034=CARTESIAN_POINT('',(4.92952879918449,1.53418275101939,0.9));
#7035=CARTESIAN_POINT('Origin',(5.,-1.8,0.3));
#7036=CARTESIAN_POINT('',(4.725,-1.8,0.4));
#7037=CARTESIAN_POINT('Origin',(5.,-1.8,0.4));
#7038=CARTESIAN_POINT('',(4.725,-1.8,1.4));
#7039=CARTESIAN_POINT('',(4.725,-1.8,0.3));
#7040=CARTESIAN_POINT('Origin',(5.,-1.8,1.4));
#7041=CARTESIAN_POINT('Origin',(5.,-1.8,1.4));
#7042=CARTESIAN_POINT('Origin',(5.,1.8,0.3));
#7043=CARTESIAN_POINT('',(4.725,1.8,0.4));
#7044=CARTESIAN_POINT('Origin',(5.,1.8,0.4));
#7045=CARTESIAN_POINT('',(4.725,1.8,1.4));
#7046=CARTESIAN_POINT('',(4.725,1.8,0.3));
#7047=CARTESIAN_POINT('Origin',(5.,1.8,1.4));
#7048=CARTESIAN_POINT('Origin',(5.,1.8,1.4));
#7049=CARTESIAN_POINT('Origin',(5.,2.8,0.3));
#7050=CARTESIAN_POINT('',(4.725,2.8,0.4));
#7051=CARTESIAN_POINT('Origin',(5.,2.8,0.4));
#7052=CARTESIAN_POINT('',(4.725,2.8,1.4));
#7053=CARTESIAN_POINT('',(4.725,2.8,0.3));
#7054=CARTESIAN_POINT('Origin',(5.,2.8,1.4));
#7055=CARTESIAN_POINT('Origin',(5.,-2.8,0.3));
#7056=CARTESIAN_POINT('',(4.725,-2.8,0.4));
#7057=CARTESIAN_POINT('Origin',(5.,-2.8,0.4));
#7058=CARTESIAN_POINT('',(4.725,-2.8,1.4));
#7059=CARTESIAN_POINT('',(4.725,-2.8,0.3));
#7060=CARTESIAN_POINT('Origin',(5.,-2.8,1.4));
#7061=CARTESIAN_POINT('Origin',(6.,3.6,0.4));
#7062=CARTESIAN_POINT('',(6.,3.6,0.4));
#7063=CARTESIAN_POINT('',(4.,3.6,0.4));
#7064=CARTESIAN_POINT('',(6.,3.6,0.4));
#7065=CARTESIAN_POINT('',(4.,3.6,1.4));
#7066=CARTESIAN_POINT('',(4.,3.6,0.4));
#7067=CARTESIAN_POINT('',(6.,3.6,1.4));
#7068=CARTESIAN_POINT('',(6.,3.6,1.4));
#7069=CARTESIAN_POINT('',(6.,3.6,0.4));
#7070=CARTESIAN_POINT('Origin',(6.,-3.6,0.4));
#7071=CARTESIAN_POINT('',(6.,-3.6,0.4));
#7072=CARTESIAN_POINT('',(6.,-3.6,0.4));
#7073=CARTESIAN_POINT('',(6.,-3.6,1.4));
#7074=CARTESIAN_POINT('',(6.,-3.6,1.4));
#7075=CARTESIAN_POINT('',(6.,-3.6,0.4));
#7076=CARTESIAN_POINT('Origin',(4.,-3.6,0.4));
#7077=CARTESIAN_POINT('',(4.,-3.6,0.4));
#7078=CARTESIAN_POINT('',(4.,-3.6,0.4));
#7079=CARTESIAN_POINT('',(4.,-3.6,1.4));
#7080=CARTESIAN_POINT('',(4.,-3.6,1.4));
#7081=CARTESIAN_POINT('',(4.,-3.6,0.4));
#7082=CARTESIAN_POINT('Origin',(4.,3.6,0.4));
#7083=CARTESIAN_POINT('',(4.,3.6,0.4));
#7084=CARTESIAN_POINT('',(4.,3.6,1.4));
#7085=CARTESIAN_POINT('Origin',(5.,0.,1.4));
#7086=CARTESIAN_POINT('Origin',(5.,0.,0.4));
#7087=CARTESIAN_POINT('',(0.,0.,0.));
#7088=CARTESIAN_POINT('Origin',(5.,0.,1.3));
#7089=CARTESIAN_POINT('',(4.85,-1.83697019872103E-17,1.4));
#7090=CARTESIAN_POINT('Origin',(5.,0.,1.4));
#7091=CARTESIAN_POINT('',(4.85,1.83697019872103E-17,1.9));
#7092=CARTESIAN_POINT('',(4.85,-1.83697019872103E-17,1.3));
#7093=CARTESIAN_POINT('Origin',(5.,0.,1.9));
#7094=CARTESIAN_POINT('Origin',(-5.,0.,1.3));
#7095=CARTESIAN_POINT('',(-5.15,-1.83697019872103E-17,1.4));
#7096=CARTESIAN_POINT('Origin',(-5.,0.,1.4));
#7097=CARTESIAN_POINT('',(-5.15,1.83697019872103E-17,1.9));
#7098=CARTESIAN_POINT('',(-5.15,-1.83697019872103E-17,1.3));
#7099=CARTESIAN_POINT('Origin',(-5.,0.,1.9));
#7100=CARTESIAN_POINT('Origin',(4.5,-1.4,1.3));
#7101=CARTESIAN_POINT('',(4.275,-1.4,1.4));
#7102=CARTESIAN_POINT('Origin',(4.5,-1.4,1.4));
#7103=CARTESIAN_POINT('',(4.275,-1.4,1.9));
#7104=CARTESIAN_POINT('',(4.275,-1.4,1.3));
#7105=CARTESIAN_POINT('Origin',(4.5,-1.4,1.9));
#7106=CARTESIAN_POINT('Origin',(-4.5,-1.4,1.3));
#7107=CARTESIAN_POINT('',(-4.725,-1.4,1.4));
#7108=CARTESIAN_POINT('Origin',(-4.5,-1.4,1.4));
#7109=CARTESIAN_POINT('',(-4.725,-1.4,1.9));
#7110=CARTESIAN_POINT('',(-4.725,-1.4,1.3));
#7111=CARTESIAN_POINT('Origin',(-4.5,-1.4,1.9));
#7112=CARTESIAN_POINT('Origin',(-4.5,1.4,1.3));
#7113=CARTESIAN_POINT('',(-4.725,1.4,1.4));
#7114=CARTESIAN_POINT('Origin',(-4.5,1.4,1.4));
#7115=CARTESIAN_POINT('',(-4.725,1.4,1.9));
#7116=CARTESIAN_POINT('',(-4.725,1.4,1.3));
#7117=CARTESIAN_POINT('Origin',(-4.5,1.4,1.9));
#7118=CARTESIAN_POINT('Origin',(0.,-1.4,1.3));
#7119=CARTESIAN_POINT('',(-0.225,-1.4,1.4));
#7120=CARTESIAN_POINT('Origin',(0.,-1.4,1.4));
#7121=CARTESIAN_POINT('',(-0.225,-1.4,1.9));
#7122=CARTESIAN_POINT('',(-0.225,-1.4,1.3));
#7123=CARTESIAN_POINT('Origin',(0.,-1.4,1.9));
#7124=CARTESIAN_POINT('Origin',(0.,1.4,1.3));
#7125=CARTESIAN_POINT('',(-0.225,1.4,1.4));
#7126=CARTESIAN_POINT('Origin',(0.,1.4,1.4));
#7127=CARTESIAN_POINT('',(-0.225,1.4,1.9));
#7128=CARTESIAN_POINT('',(-0.225,1.4,1.3));
#7129=CARTESIAN_POINT('Origin',(0.,1.4,1.9));
#7130=CARTESIAN_POINT('Origin',(4.5,1.4,1.3));
#7131=CARTESIAN_POINT('',(4.275,1.4,1.4));
#7132=CARTESIAN_POINT('Origin',(4.5,1.4,1.4));
#7133=CARTESIAN_POINT('',(4.275,1.4,1.9));
#7134=CARTESIAN_POINT('',(4.275,1.4,1.3));
#7135=CARTESIAN_POINT('Origin',(4.5,1.4,1.9));
#7136=CARTESIAN_POINT('Origin',(5.,-1.8,1.3));
#7137=CARTESIAN_POINT('',(4.79,-1.8,1.4));
#7138=CARTESIAN_POINT('Origin',(5.,-1.8,1.4));
#7139=CARTESIAN_POINT('',(4.79,-1.8,1.9));
#7140=CARTESIAN_POINT('',(4.79,-1.8,1.3));
#7141=CARTESIAN_POINT('Origin',(5.,-1.8,1.9));
#7142=CARTESIAN_POINT('Origin',(-5.,1.8,1.3));
#7143=CARTESIAN_POINT('',(-5.21,1.8,1.4));
#7144=CARTESIAN_POINT('Origin',(-5.,1.8,1.4));
#7145=CARTESIAN_POINT('',(-5.21,1.8,1.9));
#7146=CARTESIAN_POINT('',(-5.21,1.8,1.3));
#7147=CARTESIAN_POINT('Origin',(-5.,1.8,1.9));
#7148=CARTESIAN_POINT('Origin',(-5.,-1.8,1.3));
#7149=CARTESIAN_POINT('',(-5.21,-1.8,1.4));
#7150=CARTESIAN_POINT('Origin',(-5.,-1.8,1.4));
#7151=CARTESIAN_POINT('',(-5.21,-1.8,1.9));
#7152=CARTESIAN_POINT('',(-5.21,-1.8,1.3));
#7153=CARTESIAN_POINT('Origin',(-5.,-1.8,1.9));
#7154=CARTESIAN_POINT('Origin',(5.,1.8,1.3));
#7155=CARTESIAN_POINT('',(4.79,1.8,1.4));
#7156=CARTESIAN_POINT('Origin',(5.,1.8,1.4));
#7157=CARTESIAN_POINT('',(4.79,1.8,1.9));
#7158=CARTESIAN_POINT('',(4.79,1.8,1.3));
#7159=CARTESIAN_POINT('Origin',(5.,1.8,1.9));
#7160=CARTESIAN_POINT('Origin',(6.,2.25,1.4));
#7161=CARTESIAN_POINT('',(6.,2.25,1.4));
#7162=CARTESIAN_POINT('',(-6.,2.25,1.4));
#7163=CARTESIAN_POINT('',(6.,2.25,1.4));
#7164=CARTESIAN_POINT('',(-6.,2.25,1.9));
#7165=CARTESIAN_POINT('',(-6.,2.25,1.4));
#7166=CARTESIAN_POINT('',(6.,2.25,1.9));
#7167=CARTESIAN_POINT('',(6.,2.25,1.9));
#7168=CARTESIAN_POINT('',(6.,2.25,1.4));
#7169=CARTESIAN_POINT('Origin',(6.,-2.25,1.4));
#7170=CARTESIAN_POINT('',(6.,-2.25,1.4));
#7171=CARTESIAN_POINT('',(6.,-2.25,1.4));
#7172=CARTESIAN_POINT('',(6.,-2.25,1.9));
#7173=CARTESIAN_POINT('',(6.,-2.25,1.9));
#7174=CARTESIAN_POINT('',(6.,-2.25,1.4));
#7175=CARTESIAN_POINT('Origin',(-6.,-2.25,1.4));
#7176=CARTESIAN_POINT('',(-6.,-2.25,1.4));
#7177=CARTESIAN_POINT('',(-6.,-2.25,1.4));
#7178=CARTESIAN_POINT('',(-6.,-2.25,1.9));
#7179=CARTESIAN_POINT('',(-6.,-2.25,1.9));
#7180=CARTESIAN_POINT('',(-6.,-2.25,1.4));
#7181=CARTESIAN_POINT('Origin',(-6.,2.25,1.4));
#7182=CARTESIAN_POINT('',(-6.,2.25,1.4));
#7183=CARTESIAN_POINT('',(-6.,2.25,1.9));
#7184=CARTESIAN_POINT('Origin',(0.,0.,1.9));
#7185=CARTESIAN_POINT('Origin',(0.,0.,1.4));
#7186=CARTESIAN_POINT('',(0.,0.,0.));
#7187=CARTESIAN_POINT('Origin',(5.,0.,1.3));
#7188=CARTESIAN_POINT('',(4.85,-1.83697019872103E-17,1.9));
#7189=CARTESIAN_POINT('Origin',(5.,0.,1.9));
#7190=CARTESIAN_POINT('',(4.85,1.83697019872103E-17,2.));
#7191=CARTESIAN_POINT('',(4.85,-1.83697019872103E-17,1.3));
#7192=CARTESIAN_POINT('Origin',(5.,0.,2.));
#7193=CARTESIAN_POINT('Origin',(-5.,0.,1.3));
#7194=CARTESIAN_POINT('',(-5.15,-1.83697019872103E-17,1.9));
#7195=CARTESIAN_POINT('Origin',(-5.,0.,1.9));
#7196=CARTESIAN_POINT('',(-5.15,1.83697019872103E-17,2.));
#7197=CARTESIAN_POINT('',(-5.15,-1.83697019872103E-17,1.3));
#7198=CARTESIAN_POINT('Origin',(-5.,0.,2.));
#7199=CARTESIAN_POINT('Origin',(4.5,-1.4,1.3));
#7200=CARTESIAN_POINT('',(4.275,-1.4,1.9));
#7201=CARTESIAN_POINT('Origin',(4.5,-1.4,1.9));
#7202=CARTESIAN_POINT('',(4.275,-1.4,2.));
#7203=CARTESIAN_POINT('',(4.275,-1.4,1.3));
#7204=CARTESIAN_POINT('Origin',(4.5,-1.4,2.));
#7205=CARTESIAN_POINT('Origin',(-4.5,-1.4,1.3));
#7206=CARTESIAN_POINT('',(-4.725,-1.4,1.9));
#7207=CARTESIAN_POINT('Origin',(-4.5,-1.4,1.9));
#7208=CARTESIAN_POINT('',(-4.725,-1.4,2.));
#7209=CARTESIAN_POINT('',(-4.725,-1.4,1.3));
#7210=CARTESIAN_POINT('Origin',(-4.5,-1.4,2.));
#7211=CARTESIAN_POINT('Origin',(-4.5,1.4,1.3));
#7212=CARTESIAN_POINT('',(-4.725,1.4,1.9));
#7213=CARTESIAN_POINT('Origin',(-4.5,1.4,1.9));
#7214=CARTESIAN_POINT('',(-4.725,1.4,2.));
#7215=CARTESIAN_POINT('',(-4.725,1.4,1.3));
#7216=CARTESIAN_POINT('Origin',(-4.5,1.4,2.));
#7217=CARTESIAN_POINT('Origin',(0.,-1.4,1.3));
#7218=CARTESIAN_POINT('',(-0.225,-1.4,1.9));
#7219=CARTESIAN_POINT('Origin',(0.,-1.4,1.9));
#7220=CARTESIAN_POINT('',(-0.225,-1.4,2.));
#7221=CARTESIAN_POINT('',(-0.225,-1.4,1.3));
#7222=CARTESIAN_POINT('Origin',(0.,-1.4,2.));
#7223=CARTESIAN_POINT('Origin',(0.,1.4,1.3));
#7224=CARTESIAN_POINT('',(-0.225,1.4,1.9));
#7225=CARTESIAN_POINT('Origin',(0.,1.4,1.9));
#7226=CARTESIAN_POINT('',(-0.225,1.4,2.));
#7227=CARTESIAN_POINT('',(-0.225,1.4,1.3));
#7228=CARTESIAN_POINT('Origin',(0.,1.4,2.));
#7229=CARTESIAN_POINT('Origin',(4.5,1.4,1.3));
#7230=CARTESIAN_POINT('',(4.275,1.4,1.9));
#7231=CARTESIAN_POINT('Origin',(4.5,1.4,1.9));
#7232=CARTESIAN_POINT('',(4.275,1.4,2.));
#7233=CARTESIAN_POINT('',(4.275,1.4,1.3));
#7234=CARTESIAN_POINT('Origin',(4.5,1.4,2.));
#7235=CARTESIAN_POINT('Origin',(-4.,-0.8,1.8));
#7236=CARTESIAN_POINT('',(4.,-0.8,2.));
#7237=CARTESIAN_POINT('',(-4.,-0.8,2.));
#7238=CARTESIAN_POINT('',(-2.,-0.8,2.));
#7239=CARTESIAN_POINT('',(4.,-0.8,1.9));
#7240=CARTESIAN_POINT('',(4.,-0.8,1.8));
#7241=CARTESIAN_POINT('',(-4.,-0.8,1.9));
#7242=CARTESIAN_POINT('',(-2.,-0.8,1.9));
#7243=CARTESIAN_POINT('',(-4.,-0.8,1.8));
#7244=CARTESIAN_POINT('Origin',(-4.,0.8,1.8));
#7245=CARTESIAN_POINT('',(-4.,0.8,2.));
#7246=CARTESIAN_POINT('',(-4.,0.4,2.));
#7247=CARTESIAN_POINT('',(-4.,0.8,1.9));
#7248=CARTESIAN_POINT('',(-4.,0.4,1.9));
#7249=CARTESIAN_POINT('',(-4.,0.8,1.8));
#7250=CARTESIAN_POINT('Origin',(4.,0.8,1.8));
#7251=CARTESIAN_POINT('',(4.,0.8,2.));
#7252=CARTESIAN_POINT('',(2.,0.8,2.));
#7253=CARTESIAN_POINT('',(4.,0.8,1.9));
#7254=CARTESIAN_POINT('',(2.,0.8,1.9));
#7255=CARTESIAN_POINT('',(4.,0.8,1.8));
#7256=CARTESIAN_POINT('Origin',(4.,-0.8,1.8));
#7257=CARTESIAN_POINT('',(4.,-0.4,2.));
#7258=CARTESIAN_POINT('',(4.,-0.4,1.9));
#7259=CARTESIAN_POINT('Origin',(5.5,1.75,1.9));
#7260=CARTESIAN_POINT('',(5.5,1.75,1.9));
#7261=CARTESIAN_POINT('',(-5.5,1.75,1.9));
#7262=CARTESIAN_POINT('',(5.5,1.75,1.9));
#7263=CARTESIAN_POINT('',(-5.5,1.75,2.));
#7264=CARTESIAN_POINT('',(-5.5,1.75,1.9));
#7265=CARTESIAN_POINT('',(5.5,1.75,2.));
#7266=CARTESIAN_POINT('',(5.5,1.75,2.));
#7267=CARTESIAN_POINT('',(5.5,1.75,1.9));
#7268=CARTESIAN_POINT('Origin',(5.5,-1.75,1.9));
#7269=CARTESIAN_POINT('',(5.5,-1.75,1.9));
#7270=CARTESIAN_POINT('',(5.5,-1.75,1.9));
#7271=CARTESIAN_POINT('',(5.5,-1.75,2.));
#7272=CARTESIAN_POINT('',(5.5,-1.75,2.));
#7273=CARTESIAN_POINT('',(5.5,-1.75,1.9));
#7274=CARTESIAN_POINT('Origin',(-5.5,-1.75,1.9));
#7275=CARTESIAN_POINT('',(-5.5,-1.75,1.9));
#7276=CARTESIAN_POINT('',(-5.5,-1.75,1.9));
#7277=CARTESIAN_POINT('',(-5.5,-1.75,2.));
#7278=CARTESIAN_POINT('',(-5.5,-1.75,2.));
#7279=CARTESIAN_POINT('',(-5.5,-1.75,1.9));
#7280=CARTESIAN_POINT('Origin',(-5.5,1.75,1.9));
#7281=CARTESIAN_POINT('',(-5.5,1.75,1.9));
#7282=CARTESIAN_POINT('',(-5.5,1.75,2.));
#7283=CARTESIAN_POINT('Origin',(0.,0.,2.));
#7284=CARTESIAN_POINT('Origin',(0.,0.,1.9));
#7285=CARTESIAN_POINT('',(0.,0.,0.));
#7286=CARTESIAN_POINT('Origin',(-4.5,-1.8,4.));
#7287=CARTESIAN_POINT('',(-4.665,-1.75,4.));
#7288=CARTESIAN_POINT('Origin',(-4.5,-1.75,4.));
#7289=CARTESIAN_POINT('',(-4.665,-0.8,4.));
#7290=CARTESIAN_POINT('',(-4.665,-1.8,4.));
#7291=CARTESIAN_POINT('Origin',(-4.5,-0.8,4.));
#7292=CARTESIAN_POINT('Origin',(-4.5,-0.8,4.));
#7293=CARTESIAN_POINT('Origin',(4.5,-1.8,4.));
#7294=CARTESIAN_POINT('',(4.335,-1.75,4.));
#7295=CARTESIAN_POINT('Origin',(4.5,-1.75,4.));
#7296=CARTESIAN_POINT('',(4.335,-0.8,4.));
#7297=CARTESIAN_POINT('',(4.335,-1.8,4.));
#7298=CARTESIAN_POINT('Origin',(4.5,-0.8,4.));
#7299=CARTESIAN_POINT('Origin',(4.5,-0.8,4.));
#7300=CARTESIAN_POINT('Origin',(5.,0.,1.3));
#7301=CARTESIAN_POINT('',(4.85,-1.83697019872103E-17,2.));
#7302=CARTESIAN_POINT('Origin',(5.,0.,2.));
#7303=CARTESIAN_POINT('',(4.85,-1.83697019872103E-17,2.4));
#7304=CARTESIAN_POINT('',(4.85,-1.83697019872103E-17,1.3));
#7305=CARTESIAN_POINT('Origin',(5.,0.,2.4));
#7306=CARTESIAN_POINT('Origin',(5.,0.,2.4));
#7307=CARTESIAN_POINT('Origin',(-5.,0.,1.3));
#7308=CARTESIAN_POINT('',(-5.15,-1.83697019872103E-17,2.));
#7309=CARTESIAN_POINT('Origin',(-5.,0.,2.));
#7310=CARTESIAN_POINT('',(-5.15,-1.83697019872103E-17,2.4));
#7311=CARTESIAN_POINT('',(-5.15,-1.83697019872103E-17,1.3));
#7312=CARTESIAN_POINT('Origin',(-5.,0.,2.4));
#7313=CARTESIAN_POINT('Origin',(-5.,0.,2.4));
#7314=CARTESIAN_POINT('Origin',(4.5,-1.4,1.9));
#7315=CARTESIAN_POINT('',(4.335,-1.4,2.));
#7316=CARTESIAN_POINT('Origin',(4.5,-1.4,2.));
#7317=CARTESIAN_POINT('',(4.335,-1.4,3.2));
#7318=CARTESIAN_POINT('',(4.335,-1.4,1.9));
#7319=CARTESIAN_POINT('Origin',(4.5,-1.4,3.2));
#7320=CARTESIAN_POINT('Origin',(4.5,-1.4,3.2));
#7321=CARTESIAN_POINT('Origin',(-4.5,-1.4,1.9));
#7322=CARTESIAN_POINT('',(-4.665,-1.4,2.));
#7323=CARTESIAN_POINT('Origin',(-4.5,-1.4,2.));
#7324=CARTESIAN_POINT('',(-4.665,-1.4,3.2));
#7325=CARTESIAN_POINT('',(-4.665,-1.4,1.9));
#7326=CARTESIAN_POINT('Origin',(-4.5,-1.4,3.2));
#7327=CARTESIAN_POINT('Origin',(-4.5,-1.4,3.2));
#7328=CARTESIAN_POINT('Origin',(-4.5,1.4,1.9));
#7329=CARTESIAN_POINT('',(-4.665,1.4,2.));
#7330=CARTESIAN_POINT('Origin',(-4.5,1.4,2.));
#7331=CARTESIAN_POINT('',(-4.665,1.4,3.2));
#7332=CARTESIAN_POINT('',(-4.665,1.4,1.9));
#7333=CARTESIAN_POINT('Origin',(-4.5,1.4,3.2));
#7334=CARTESIAN_POINT('Origin',(-4.5,1.4,3.2));
#7335=CARTESIAN_POINT('Origin',(0.,-1.4,1.9));
#7336=CARTESIAN_POINT('',(-0.165,-1.4,2.));
#7337=CARTESIAN_POINT('Origin',(0.,-1.4,2.));
#7338=CARTESIAN_POINT('',(-0.165,-1.4,3.2));
#7339=CARTESIAN_POINT('',(-0.165,-1.4,1.9));
#7340=CARTESIAN_POINT('Origin',(0.,-1.4,3.2));
#7341=CARTESIAN_POINT('Origin',(0.,-1.4,3.2));
#7342=CARTESIAN_POINT('Origin',(0.,1.4,1.9));
#7343=CARTESIAN_POINT('',(-0.165,1.4,2.));
#7344=CARTESIAN_POINT('Origin',(0.,1.4,2.));
#7345=CARTESIAN_POINT('',(-0.165,1.4,3.2));
#7346=CARTESIAN_POINT('',(-0.165,1.4,1.9));
#7347=CARTESIAN_POINT('Origin',(0.,1.4,3.2));
#7348=CARTESIAN_POINT('Origin',(0.,1.4,3.2));
#7349=CARTESIAN_POINT('Origin',(4.5,1.4,1.9));
#7350=CARTESIAN_POINT('',(4.335,1.4,2.));
#7351=CARTESIAN_POINT('Origin',(4.5,1.4,2.));
#7352=CARTESIAN_POINT('',(4.335,1.4,3.2));
#7353=CARTESIAN_POINT('',(4.335,1.4,1.9));
#7354=CARTESIAN_POINT('Origin',(4.5,1.4,3.2));
#7355=CARTESIAN_POINT('Origin',(4.5,1.4,3.2));
#7356=CARTESIAN_POINT('Origin',(4.1,0.,3.5));
#7357=CARTESIAN_POINT('',(4.1,-8.38883057415937E-17,4.185));
#7358=CARTESIAN_POINT('Origin',(4.1,0.,3.5));
#7359=CARTESIAN_POINT('',(5.5,8.38883057415937E-17,4.185));
#7360=CARTESIAN_POINT('',(4.1,-8.38883057415937E-17,4.185));
#7361=CARTESIAN_POINT('Origin',(5.5,0.,3.5));
#7362=CARTESIAN_POINT('Origin',(4.1,0.,3.5));
#7363=CARTESIAN_POINT('',(4.1,-3.67394039744206E-17,3.8));
#7364=CARTESIAN_POINT('Origin',(4.1,0.,3.5));
#7365=CARTESIAN_POINT('Origin',(-5.6,0.,3.5));
#7366=CARTESIAN_POINT('',(-5.5,-8.38883057415937E-17,4.185));
#7367=CARTESIAN_POINT('Origin',(-5.5,0.,3.5));
#7368=CARTESIAN_POINT('',(-4.1,-8.38883057415937E-17,4.185));
#7369=CARTESIAN_POINT('',(-5.6,-8.38883057415937E-17,4.185));
#7370=CARTESIAN_POINT('Origin',(-4.1,0.,3.5));
#7371=CARTESIAN_POINT('Origin',(-4.1,0.,3.5));
#7372=CARTESIAN_POINT('',(-4.1,3.67394039744206E-17,3.8));
#7373=CARTESIAN_POINT('Origin',(-4.1,0.,3.5));
#7374=CARTESIAN_POINT('Origin',(3.75,0.,3.4));
#7375=CARTESIAN_POINT('',(3.75,-0.2,3.72360679774998));
#7376=CARTESIAN_POINT('',(3.95,1.4590044056349E-17,3.8));
#7377=CARTESIAN_POINT('Ctrl Pts',(3.75,-0.2,3.72360679774998));
#7378=CARTESIAN_POINT('Ctrl Pts',(3.77630182346442,-0.2,3.72360679774998));
#7379=CARTESIAN_POINT('Ctrl Pts',(3.80333179602069,-0.194568877616075,3.72872056892082));
#7380=CARTESIAN_POINT('Ctrl Pts',(3.85213335089966,-0.173983137835284,3.74474475389314));
#7381=CARTESIAN_POINT('Ctrl Pts',(3.87402433525872,-0.158818377215904,3.75527603224183));
#7382=CARTESIAN_POINT('Ctrl Pts',(3.90862698590243,-0.124215726572194,3.77377192701083));
#7383=CARTESIAN_POINT('Ctrl Pts',(3.92391823287771,-0.102283014436697,3.78316729552365));
#7384=CARTESIAN_POINT('Ctrl Pts',(3.94462445314031,-0.0532042473651336,
3.79633569102376));
#7385=CARTESIAN_POINT('Ctrl Pts',(3.95,-0.0260124669966692,3.8));
#7386=CARTESIAN_POINT('Ctrl Pts',(3.95,9.71445146547012E-17,3.8));
#7387=CARTESIAN_POINT('',(3.55,-2.43895323233112E-17,3.8));
#7388=CARTESIAN_POINT('Ctrl Pts',(3.55,-2.77555756156289E-17,3.8));
#7389=CARTESIAN_POINT('Ctrl Pts',(3.55,-0.0260124669966693,3.8));
#7390=CARTESIAN_POINT('Ctrl Pts',(3.55537554685969,-0.0532042473651339,
3.79633569102376));
#7391=CARTESIAN_POINT('Ctrl Pts',(3.57608176712229,-0.102283014436697,3.78316729552365));
#7392=CARTESIAN_POINT('Ctrl Pts',(3.59137301409757,-0.124215726572194,3.77377192701083));
#7393=CARTESIAN_POINT('Ctrl Pts',(3.62597566474128,-0.158818377215904,3.75527603224183));
#7394=CARTESIAN_POINT('Ctrl Pts',(3.64786664910034,-0.173983137835283,3.74474475389314));
#7395=CARTESIAN_POINT('Ctrl Pts',(3.69666820397931,-0.194568877616075,3.72872056892082));
#7396=CARTESIAN_POINT('Ctrl Pts',(3.72369817653558,-0.2,3.72360679774998));
#7397=CARTESIAN_POINT('Ctrl Pts',(3.75,-0.2,3.72360679774998));
#7398=CARTESIAN_POINT('',(3.55,2.44929359829471E-17,4.35));
#7399=CARTESIAN_POINT('',(3.55,-2.44929359829471E-17,3.4));
#7400=CARTESIAN_POINT('Origin',(3.75,0.,4.35));
#7401=CARTESIAN_POINT('Ctrl Pts',(3.95,6.24500451351651E-17,3.8));
#7402=CARTESIAN_POINT('Ctrl Pts',(3.95,0.0260124669966693,3.8));
#7403=CARTESIAN_POINT('Ctrl Pts',(3.94462445314031,0.0532042473651336,3.79633569102376));
#7404=CARTESIAN_POINT('Ctrl Pts',(3.92391823287771,0.102283014436697,3.78316729552365));
#7405=CARTESIAN_POINT('Ctrl Pts',(3.90862698590243,0.124215726572194,3.77377192701083));
#7406=CARTESIAN_POINT('Ctrl Pts',(3.87402433525872,0.158818377215904,3.75527603224183));
#7407=CARTESIAN_POINT('Ctrl Pts',(3.85213335089966,0.173983137835284,3.74474475389314));
#7408=CARTESIAN_POINT('Ctrl Pts',(3.80333179602069,0.194568877616075,3.72872056892082));
#7409=CARTESIAN_POINT('Ctrl Pts',(3.77630182346442,0.2,3.72360679774998));
#7410=CARTESIAN_POINT('Ctrl Pts',(3.72369817653558,0.2,3.72360679774998));
#7411=CARTESIAN_POINT('Ctrl Pts',(3.69666820397931,0.194568877616075,3.72872056892082));
#7412=CARTESIAN_POINT('Ctrl Pts',(3.64786664910035,0.173983137835284,3.74474475389314));
#7413=CARTESIAN_POINT('Ctrl Pts',(3.62597566474128,0.158818377215904,3.75527603224183));
#7414=CARTESIAN_POINT('Ctrl Pts',(3.59137301409757,0.124215726572194,3.77377192701083));
#7415=CARTESIAN_POINT('Ctrl Pts',(3.57608176712229,0.102283014436697,3.78316729552365));
#7416=CARTESIAN_POINT('Ctrl Pts',(3.55537554685969,0.0532042473651339,3.79633569102376));
#7417=CARTESIAN_POINT('Ctrl Pts',(3.55,0.0260124669966693,3.8));
#7418=CARTESIAN_POINT('Ctrl Pts',(3.55,-2.77555756156289E-17,3.8));
#7419=CARTESIAN_POINT('Origin',(3.75,0.,4.35));
#7420=CARTESIAN_POINT('',(3.235,-6.30693101560886E-17,4.35));
#7421=CARTESIAN_POINT('Origin',(3.75,0.,4.35));
#7422=CARTESIAN_POINT('',(3.235,6.30693101560886E-17,5.));
#7423=CARTESIAN_POINT('',(3.235,-6.30693101560886E-17,4.35));
#7424=CARTESIAN_POINT('Origin',(3.75,0.,5.));
#7425=CARTESIAN_POINT('Origin',(3.75,0.,4.35));
#7426=CARTESIAN_POINT('Origin',(1.25,0.,3.4));
#7427=CARTESIAN_POINT('',(1.25,-0.2,3.72360679774998));
#7428=CARTESIAN_POINT('',(1.45,-1.02246722744222E-18,3.8));
#7429=CARTESIAN_POINT('Ctrl Pts',(1.25,-0.2,3.72360679774998));
#7430=CARTESIAN_POINT('Ctrl Pts',(1.27630182346442,-0.2,3.72360679774998));
#7431=CARTESIAN_POINT('Ctrl Pts',(1.30333179602069,-0.194568877616075,3.72872056892082));
#7432=CARTESIAN_POINT('Ctrl Pts',(1.35213335089965,-0.173983137835284,3.74474475389314));
#7433=CARTESIAN_POINT('Ctrl Pts',(1.37402433525871,-0.158818377215904,3.75527603224183));
#7434=CARTESIAN_POINT('Ctrl Pts',(1.40862698590242,-0.124215726572194,3.77377192701083));
#7435=CARTESIAN_POINT('Ctrl Pts',(1.42391823287771,-0.102283014436697,3.78316729552365));
#7436=CARTESIAN_POINT('Ctrl Pts',(1.44462445314031,-0.0532042473651338,
3.79633569102376));
#7437=CARTESIAN_POINT('Ctrl Pts',(1.45,-0.0260124669966693,3.8));
#7438=CARTESIAN_POINT('Ctrl Pts',(1.45,3.46944695195361E-17,3.8));
#7439=CARTESIAN_POINT('',(1.05,-2.6124255799288E-17,3.8));
#7440=CARTESIAN_POINT('Ctrl Pts',(1.05,-2.08166817117217E-17,3.8));
#7441=CARTESIAN_POINT('Ctrl Pts',(1.05,-0.0260124669966693,3.8));
#7442=CARTESIAN_POINT('Ctrl Pts',(1.05537554685969,-0.0532042473651339,
3.79633569102376));
#7443=CARTESIAN_POINT('Ctrl Pts',(1.07608176712229,-0.102283014436697,3.78316729552365));
#7444=CARTESIAN_POINT('Ctrl Pts',(1.09137301409758,-0.124215726572194,3.77377192701083));
#7445=CARTESIAN_POINT('Ctrl Pts',(1.12597566474129,-0.158818377215904,3.75527603224183));
#7446=CARTESIAN_POINT('Ctrl Pts',(1.14786664910035,-0.173983137835284,3.74474475389314));
#7447=CARTESIAN_POINT('Ctrl Pts',(1.19666820397931,-0.194568877616075,3.72872056892082));
#7448=CARTESIAN_POINT('Ctrl Pts',(1.22369817653558,-0.2,3.72360679774998));
#7449=CARTESIAN_POINT('Ctrl Pts',(1.25,-0.2,3.72360679774998));
#7450=CARTESIAN_POINT('',(1.05,2.44929359829471E-17,4.35));
#7451=CARTESIAN_POINT('',(1.05,-2.44929359829471E-17,3.4));
#7452=CARTESIAN_POINT('Origin',(1.25,0.,4.35));
#7453=CARTESIAN_POINT('Ctrl Pts',(1.45,2.77555756156289E-17,3.8));
#7454=CARTESIAN_POINT('Ctrl Pts',(1.45,0.0260124669966693,3.8));
#7455=CARTESIAN_POINT('Ctrl Pts',(1.44462445314031,0.0532042473651337,3.79633569102376));
#7456=CARTESIAN_POINT('Ctrl Pts',(1.42391823287771,0.102283014436697,3.78316729552365));
#7457=CARTESIAN_POINT('Ctrl Pts',(1.40862698590243,0.124215726572194,3.77377192701083));
#7458=CARTESIAN_POINT('Ctrl Pts',(1.37402433525872,0.158818377215904,3.75527603224183));
#7459=CARTESIAN_POINT('Ctrl Pts',(1.35213335089966,0.173983137835283,3.74474475389314));
#7460=CARTESIAN_POINT('Ctrl Pts',(1.30333179602069,0.194568877616075,3.72872056892082));
#7461=CARTESIAN_POINT('Ctrl Pts',(1.27630182346442,0.2,3.72360679774998));
#7462=CARTESIAN_POINT('Ctrl Pts',(1.22369817653558,0.2,3.72360679774998));
#7463=CARTESIAN_POINT('Ctrl Pts',(1.19666820397931,0.194568877616075,3.72872056892082));
#7464=CARTESIAN_POINT('Ctrl Pts',(1.14786664910035,0.173983137835284,3.74474475389314));
#7465=CARTESIAN_POINT('Ctrl Pts',(1.12597566474129,0.158818377215904,3.75527603224183));
#7466=CARTESIAN_POINT('Ctrl Pts',(1.09137301409758,0.124215726572194,3.77377192701083));
#7467=CARTESIAN_POINT('Ctrl Pts',(1.07608176712229,0.102283014436697,3.78316729552365));
#7468=CARTESIAN_POINT('Ctrl Pts',(1.05537554685969,0.0532042473651338,3.79633569102376));
#7469=CARTESIAN_POINT('Ctrl Pts',(1.05,0.0260124669966694,3.8));
#7470=CARTESIAN_POINT('Ctrl Pts',(1.05,4.16333634234434E-17,3.8));
#7471=CARTESIAN_POINT('Origin',(1.25,0.,4.35));
#7472=CARTESIAN_POINT('',(0.735,-6.30693101560887E-17,4.35));
#7473=CARTESIAN_POINT('Origin',(1.25,0.,4.35));
#7474=CARTESIAN_POINT('',(0.735,6.30693101560887E-17,5.));
#7475=CARTESIAN_POINT('',(0.735,-6.30693101560887E-17,4.35));
#7476=CARTESIAN_POINT('Origin',(1.25,0.,5.));
#7477=CARTESIAN_POINT('Origin',(1.25,0.,4.35));
#7478=CARTESIAN_POINT('Origin',(-1.25,0.,3.4));
#7479=CARTESIAN_POINT('',(-1.25,-0.2,3.72360679774998));
#7480=CARTESIAN_POINT('',(-1.05,-2.53085958911175E-17,3.8));
#7481=CARTESIAN_POINT('Ctrl Pts',(-1.25,-0.2,3.72360679774998));
#7482=CARTESIAN_POINT('Ctrl Pts',(-1.22369817653558,-0.2,3.72360679774998));
#7483=CARTESIAN_POINT('Ctrl Pts',(-1.19666820397931,-0.194568877616075,
3.72872056892082));
#7484=CARTESIAN_POINT('Ctrl Pts',(-1.14786664910035,-0.173983137835284,
3.74474475389314));
#7485=CARTESIAN_POINT('Ctrl Pts',(-1.12597566474129,-0.158818377215904,
3.75527603224183));
#7486=CARTESIAN_POINT('Ctrl Pts',(-1.09137301409758,-0.124215726572194,
3.77377192701083));
#7487=CARTESIAN_POINT('Ctrl Pts',(-1.07608176712229,-0.102283014436697,
3.78316729552365));
#7488=CARTESIAN_POINT('Ctrl Pts',(-1.05537554685969,-0.0532042473651338,
3.79633569102376));
#7489=CARTESIAN_POINT('Ctrl Pts',(-1.05,-0.0260124669966693,3.8));
#7490=CARTESIAN_POINT('Ctrl Pts',(-1.05,5.55111512312578E-17,3.8));
#7491=CARTESIAN_POINT('',(-1.45,-1.91853618953807E-17,3.8));
#7492=CARTESIAN_POINT('Ctrl Pts',(-1.45,-2.77555756156289E-17,3.8));
#7493=CARTESIAN_POINT('Ctrl Pts',(-1.45,-0.0260124669966693,3.8));
#7494=CARTESIAN_POINT('Ctrl Pts',(-1.44462445314031,-0.0532042473651339,
3.79633569102376));
#7495=CARTESIAN_POINT('Ctrl Pts',(-1.42391823287771,-0.102283014436697,
3.78316729552365));
#7496=CARTESIAN_POINT('Ctrl Pts',(-1.40862698590242,-0.124215726572194,
3.77377192701083));
#7497=CARTESIAN_POINT('Ctrl Pts',(-1.37402433525871,-0.158818377215904,
3.75527603224183));
#7498=CARTESIAN_POINT('Ctrl Pts',(-1.35213335089965,-0.173983137835284,
3.74474475389314));
#7499=CARTESIAN_POINT('Ctrl Pts',(-1.30333179602069,-0.194568877616075,
3.72872056892082));
#7500=CARTESIAN_POINT('Ctrl Pts',(-1.27630182346442,-0.2,3.72360679774998));
#7501=CARTESIAN_POINT('Ctrl Pts',(-1.25,-0.2,3.72360679774998));
#7502=CARTESIAN_POINT('',(-1.45,2.44929359829471E-17,4.35));
#7503=CARTESIAN_POINT('',(-1.45,-2.44929359829471E-17,3.4));
#7504=CARTESIAN_POINT('Origin',(-1.25,0.,4.35));
#7505=CARTESIAN_POINT('Ctrl Pts',(-1.05,-1.38777878078145E-17,3.8));
#7506=CARTESIAN_POINT('Ctrl Pts',(-1.05,0.0260124669966692,3.8));
#7507=CARTESIAN_POINT('Ctrl Pts',(-1.05537554685969,0.0532042473651337,
3.79633569102376));
#7508=CARTESIAN_POINT('Ctrl Pts',(-1.07608176712229,0.102283014436697,3.78316729552365));
#7509=CARTESIAN_POINT('Ctrl Pts',(-1.09137301409757,0.124215726572194,3.77377192701083));
#7510=CARTESIAN_POINT('Ctrl Pts',(-1.12597566474128,0.158818377215904,3.75527603224183));
#7511=CARTESIAN_POINT('Ctrl Pts',(-1.14786664910034,0.173983137835283,3.74474475389314));
#7512=CARTESIAN_POINT('Ctrl Pts',(-1.19666820397931,0.194568877616075,3.72872056892082));
#7513=CARTESIAN_POINT('Ctrl Pts',(-1.22369817653558,0.2,3.72360679774998));
#7514=CARTESIAN_POINT('Ctrl Pts',(-1.27630182346442,0.2,3.72360679774998));
#7515=CARTESIAN_POINT('Ctrl Pts',(-1.30333179602069,0.194568877616075,3.72872056892082));
#7516=CARTESIAN_POINT('Ctrl Pts',(-1.35213335089965,0.173983137835284,3.74474475389314));
#7517=CARTESIAN_POINT('Ctrl Pts',(-1.37402433525871,0.158818377215904,3.75527603224183));
#7518=CARTESIAN_POINT('Ctrl Pts',(-1.40862698590242,0.124215726572194,3.77377192701083));
#7519=CARTESIAN_POINT('Ctrl Pts',(-1.42391823287771,0.102283014436697,3.78316729552365));
#7520=CARTESIAN_POINT('Ctrl Pts',(-1.44462445314031,0.0532042473651338,
3.79633569102376));
#7521=CARTESIAN_POINT('Ctrl Pts',(-1.45,0.0260124669966693,3.8));
#7522=CARTESIAN_POINT('Ctrl Pts',(-1.45,-3.81639164714898E-17,3.8));
#7523=CARTESIAN_POINT('Origin',(-1.25,0.,4.35));
#7524=CARTESIAN_POINT('',(-1.765,-6.30693101560887E-17,4.35));
#7525=CARTESIAN_POINT('Origin',(-1.25,0.,4.35));
#7526=CARTESIAN_POINT('',(-1.765,6.30693101560887E-17,5.));
#7527=CARTESIAN_POINT('',(-1.765,-6.30693101560887E-17,4.35));
#7528=CARTESIAN_POINT('Origin',(-1.25,0.,5.));
#7529=CARTESIAN_POINT('Origin',(-1.25,0.,4.35));
#7530=CARTESIAN_POINT('Origin',(-3.75,0.,3.4));
#7531=CARTESIAN_POINT('',(-3.75,-0.2,3.72360679774998));
#7532=CARTESIAN_POINT('',(-3.55,4.1817032004882E-18,3.8));
#7533=CARTESIAN_POINT('Ctrl Pts',(-3.75,-0.2,3.72360679774998));
#7534=CARTESIAN_POINT('Ctrl Pts',(-3.72369817653558,-0.2,3.72360679774998));
#7535=CARTESIAN_POINT('Ctrl Pts',(-3.69666820397931,-0.194568877616075,
3.72872056892082));
#7536=CARTESIAN_POINT('Ctrl Pts',(-3.64786664910034,-0.173983137835284,
3.74474475389314));
#7537=CARTESIAN_POINT('Ctrl Pts',(-3.62597566474128,-0.158818377215904,
3.75527603224183));
#7538=CARTESIAN_POINT('Ctrl Pts',(-3.59137301409757,-0.124215726572194,
3.77377192701083));
#7539=CARTESIAN_POINT('Ctrl Pts',(-3.57608176712229,-0.102283014436697,
3.78316729552365));
#7540=CARTESIAN_POINT('Ctrl Pts',(-3.55537554685969,-0.0532042473651337,
3.79633569102376));
#7541=CARTESIAN_POINT('Ctrl Pts',(-3.55,-0.0260124669966693,3.8));
#7542=CARTESIAN_POINT('Ctrl Pts',(-3.55,6.24500451351651E-17,3.8));
#7543=CARTESIAN_POINT('',(-3.95,-2.09200853713576E-17,3.8));
#7544=CARTESIAN_POINT('Ctrl Pts',(-3.95,-1.73472347597681E-17,3.8));
#7545=CARTESIAN_POINT('Ctrl Pts',(-3.95,-0.0260124669966693,3.8));
#7546=CARTESIAN_POINT('Ctrl Pts',(-3.94462445314031,-0.0532042473651343,
3.79633569102376));
#7547=CARTESIAN_POINT('Ctrl Pts',(-3.92391823287771,-0.102283014436697,
3.78316729552365));
#7548=CARTESIAN_POINT('Ctrl Pts',(-3.90862698590243,-0.124215726572194,
3.77377192701083));
#7549=CARTESIAN_POINT('Ctrl Pts',(-3.87402433525872,-0.158818377215904,
3.75527603224183));
#7550=CARTESIAN_POINT('Ctrl Pts',(-3.85213335089965,-0.173983137835284,
3.74474475389314));
#7551=CARTESIAN_POINT('Ctrl Pts',(-3.80333179602069,-0.194568877616075,
3.72872056892082));
#7552=CARTESIAN_POINT('Ctrl Pts',(-3.77630182346442,-0.2,3.72360679774998));
#7553=CARTESIAN_POINT('Ctrl Pts',(-3.75,-0.2,3.72360679774998));
#7554=CARTESIAN_POINT('',(-3.95,2.44929359829471E-17,4.35));
#7555=CARTESIAN_POINT('',(-3.95,-2.44929359829471E-17,3.4));
#7556=CARTESIAN_POINT('Origin',(-3.75,0.,4.35));
#7557=CARTESIAN_POINT('Ctrl Pts',(-3.55,3.81639164714898E-17,3.8));
#7558=CARTESIAN_POINT('Ctrl Pts',(-3.55,0.0260124669966693,3.8));
#7559=CARTESIAN_POINT('Ctrl Pts',(-3.55537554685969,0.0532042473651338,
3.79633569102376));
#7560=CARTESIAN_POINT('Ctrl Pts',(-3.57608176712229,0.102283014436697,3.78316729552365));
#7561=CARTESIAN_POINT('Ctrl Pts',(-3.59137301409758,0.124215726572194,3.77377192701083));
#7562=CARTESIAN_POINT('Ctrl Pts',(-3.62597566474129,0.158818377215904,3.75527603224183));
#7563=CARTESIAN_POINT('Ctrl Pts',(-3.64786664910034,0.173983137835284,3.74474475389314));
#7564=CARTESIAN_POINT('Ctrl Pts',(-3.69666820397931,0.194568877616075,3.72872056892082));
#7565=CARTESIAN_POINT('Ctrl Pts',(-3.72369817653558,0.2,3.72360679774998));
#7566=CARTESIAN_POINT('Ctrl Pts',(-3.77630182346442,0.2,3.72360679774998));
#7567=CARTESIAN_POINT('Ctrl Pts',(-3.80333179602069,0.194568877616075,3.72872056892082));
#7568=CARTESIAN_POINT('Ctrl Pts',(-3.85213335089965,0.173983137835284,3.74474475389314));
#7569=CARTESIAN_POINT('Ctrl Pts',(-3.87402433525872,0.158818377215904,3.75527603224183));
#7570=CARTESIAN_POINT('Ctrl Pts',(-3.90862698590243,0.124215726572194,3.77377192701083));
#7571=CARTESIAN_POINT('Ctrl Pts',(-3.92391823287771,0.102283014436697,3.78316729552365));
#7572=CARTESIAN_POINT('Ctrl Pts',(-3.94462445314031,0.0532042473651338,
3.79633569102376));
#7573=CARTESIAN_POINT('Ctrl Pts',(-3.95,0.0260124669966692,3.8));
#7574=CARTESIAN_POINT('Ctrl Pts',(-3.95,-1.17961196366423E-16,3.8));
#7575=CARTESIAN_POINT('Origin',(-3.75,0.,4.35));
#7576=CARTESIAN_POINT('',(-4.265,-6.30693101560887E-17,4.35));
#7577=CARTESIAN_POINT('Origin',(-3.75,0.,4.35));
#7578=CARTESIAN_POINT('',(-4.265,6.30693101560887E-17,5.));
#7579=CARTESIAN_POINT('',(-4.265,-6.30693101560887E-17,4.35));
#7580=CARTESIAN_POINT('Origin',(-3.75,0.,5.));
#7581=CARTESIAN_POINT('Origin',(-3.75,0.,4.35));
#7582=CARTESIAN_POINT('Origin',(-4.,-0.8,1.9));
#7583=CARTESIAN_POINT('',(-4.,-0.8,2.));
#7584=CARTESIAN_POINT('',(4.,-0.8,2.));
#7585=CARTESIAN_POINT('',(-2.,-0.8,2.));
#7586=CARTESIAN_POINT('',(-4.,-0.8,3.5));
#7587=CARTESIAN_POINT('',(-4.,-0.8,1.9));
#7588=CARTESIAN_POINT('',(4.,-0.8,3.5));
#7589=CARTESIAN_POINT('',(-4.,-0.8,3.5));
#7590=CARTESIAN_POINT('',(4.,-0.8,1.9));
#7591=CARTESIAN_POINT('Origin',(4.,-0.8,1.9));
#7592=CARTESIAN_POINT('',(4.,0.8,2.));
#7593=CARTESIAN_POINT('',(4.,-0.4,2.));
#7594=CARTESIAN_POINT('',(4.,-0.3,3.5));
#7595=CARTESIAN_POINT('',(4.,-0.8,3.5));
#7596=CARTESIAN_POINT('',(4.,0.3,3.5));
#7597=CARTESIAN_POINT('Origin',(4.,0.,3.5));
#7598=CARTESIAN_POINT('',(4.,0.8,3.5));
#7599=CARTESIAN_POINT('',(4.,-0.8,3.5));
#7600=CARTESIAN_POINT('',(4.,0.8,1.9));
#7601=CARTESIAN_POINT('Origin',(0.,0.,3.5));
#7602=CARTESIAN_POINT('',(-4.,-0.3,3.5));
#7603=CARTESIAN_POINT('',(-5.6,-0.3,3.5));
#7604=CARTESIAN_POINT('',(-4.,0.8,3.5));
#7605=CARTESIAN_POINT('Origin',(4.,0.8,1.9));
#7606=CARTESIAN_POINT('',(-4.,0.8,2.));
#7607=CARTESIAN_POINT('',(2.,0.8,2.));
#7608=CARTESIAN_POINT('',(-4.,0.8,3.5));
#7609=CARTESIAN_POINT('',(4.,0.8,3.5));
#7610=CARTESIAN_POINT('',(-4.,0.8,1.9));
#7611=CARTESIAN_POINT('Origin',(-4.,0.8,1.9));
#7612=CARTESIAN_POINT('',(-4.,0.4,2.));
#7613=CARTESIAN_POINT('',(-4.,0.3,3.5));
#7614=CARTESIAN_POINT('',(-4.,0.8,3.5));
#7615=CARTESIAN_POINT('Origin',(-4.,0.,3.5));
#7616=CARTESIAN_POINT('Origin',(0.,0.,3.5));
#7617=CARTESIAN_POINT('',(-5.6,0.3,3.5));
#7618=CARTESIAN_POINT('Origin',(-5.6,0.,3.5));
#7619=CARTESIAN_POINT('',(-5.6,-3.67394039744206E-17,3.8));
#7620=CARTESIAN_POINT('',(-5.6,-3.67394039744206E-17,3.8));
#7621=CARTESIAN_POINT('',(-5.6,-3.67394039744206E-17,3.8));
#7622=CARTESIAN_POINT('',(-5.6,-3.67394039744206E-17,3.8));
#7623=CARTESIAN_POINT('',(-5.6,-3.67394039744206E-17,3.8));
#7624=CARTESIAN_POINT('Origin',(5.5,1.75,2.));
#7625=CARTESIAN_POINT('',(5.5,1.75,2.));
#7626=CARTESIAN_POINT('',(-5.5,1.75,2.));
#7627=CARTESIAN_POINT('',(5.5,1.75,2.));
#7628=CARTESIAN_POINT('',(-5.5,1.75,5.));
#7629=CARTESIAN_POINT('',(-5.5,1.75,2.));
#7630=CARTESIAN_POINT('',(5.5,1.75,5.));
#7631=CARTESIAN_POINT('',(5.5,1.75,5.));
#7632=CARTESIAN_POINT('',(5.5,1.75,2.));
#7633=CARTESIAN_POINT('Origin',(5.5,-1.75,2.));
#7634=CARTESIAN_POINT('',(5.5,-1.75,2.));
#7635=CARTESIAN_POINT('',(5.5,-1.75,2.));
#7636=CARTESIAN_POINT('',(5.5,-1.75,5.));
#7637=CARTESIAN_POINT('',(5.5,-1.75,5.));
#7638=CARTESIAN_POINT('',(5.5,-1.75,2.));
#7639=CARTESIAN_POINT('Origin',(-5.5,-1.75,2.));
#7640=CARTESIAN_POINT('',(-5.5,-1.75,2.));
#7641=CARTESIAN_POINT('',(-5.5,-1.75,2.));
#7642=CARTESIAN_POINT('',(-5.5,-1.75,5.));
#7643=CARTESIAN_POINT('',(-5.5,-1.75,5.));
#7644=CARTESIAN_POINT('',(-5.5,-1.75,2.));
#7645=CARTESIAN_POINT('Origin',(-5.5,1.75,2.));
#7646=CARTESIAN_POINT('',(-5.5,1.75,2.));
#7647=CARTESIAN_POINT('',(-5.5,1.75,5.));
#7648=CARTESIAN_POINT('Origin',(0.,0.,5.));
#7649=CARTESIAN_POINT('Origin',(0.,0.,2.));
#7650=CARTESIAN_POINT('',(0.,0.,0.));
#7651=CARTESIAN_POINT('Origin',(-3.75,0.,5.7));
#7652=CARTESIAN_POINT('',(-3.95,-2.44929359829471E-17,8.95));
#7653=CARTESIAN_POINT('Origin',(-3.75,0.,8.95));
#7654=CARTESIAN_POINT('',(-3.95,-2.44929359829471E-17,5.7));
#7655=CARTESIAN_POINT('',(-3.95,-2.44929359829471E-17,5.7));
#7656=CARTESIAN_POINT('Origin',(-3.75,0.,5.7));
#7657=CARTESIAN_POINT('Origin',(-3.75,0.,5.7));
#7658=CARTESIAN_POINT('',(-4.05,-3.67394039744206E-17,8.95));
#7659=CARTESIAN_POINT('Origin',(-3.75,0.,8.95));
#7660=CARTESIAN_POINT('',(-4.05,-3.67394039744206E-17,5.7));
#7661=CARTESIAN_POINT('',(-4.05,-3.67394039744206E-17,5.7));
#7662=CARTESIAN_POINT('Origin',(-3.75,0.,5.7));
#7663=CARTESIAN_POINT('Origin',(-3.75,0.,8.95));
#7664=CARTESIAN_POINT('Origin',(-3.75,0.,5.7));
#7665=CARTESIAN_POINT('',(0.,0.,0.));
#7666=CARTESIAN_POINT('Origin',(-1.25,0.,5.7));
#7667=CARTESIAN_POINT('',(-1.45,-2.44929359829471E-17,8.95));
#7668=CARTESIAN_POINT('Origin',(-1.25,0.,8.95));
#7669=CARTESIAN_POINT('',(-1.45,-2.44929359829471E-17,5.7));
#7670=CARTESIAN_POINT('',(-1.45,-2.44929359829471E-17,5.7));
#7671=CARTESIAN_POINT('Origin',(-1.25,0.,5.7));
#7672=CARTESIAN_POINT('Origin',(-1.25,0.,5.7));
#7673=CARTESIAN_POINT('',(-1.55,-3.67394039744206E-17,8.95));
#7674=CARTESIAN_POINT('Origin',(-1.25,0.,8.95));
#7675=CARTESIAN_POINT('',(-1.55,-3.67394039744206E-17,5.7));
#7676=CARTESIAN_POINT('',(-1.55,-3.67394039744206E-17,5.7));
#7677=CARTESIAN_POINT('Origin',(-1.25,0.,5.7));
#7678=CARTESIAN_POINT('Origin',(-1.25,0.,8.95));
#7679=CARTESIAN_POINT('Origin',(-1.25,0.,5.7));
#7680=CARTESIAN_POINT('',(0.,0.,0.));
#7681=CARTESIAN_POINT('Origin',(1.25,0.,5.7));
#7682=CARTESIAN_POINT('',(1.05,-2.44929359829471E-17,8.95));
#7683=CARTESIAN_POINT('Origin',(1.25,0.,8.95));
#7684=CARTESIAN_POINT('',(1.05,-2.44929359829471E-17,5.7));
#7685=CARTESIAN_POINT('',(1.05,-2.44929359829471E-17,5.7));
#7686=CARTESIAN_POINT('Origin',(1.25,0.,5.7));
#7687=CARTESIAN_POINT('Origin',(1.25,0.,5.7));
#7688=CARTESIAN_POINT('',(0.95,-3.67394039744206E-17,8.95));
#7689=CARTESIAN_POINT('Origin',(1.25,0.,8.95));
#7690=CARTESIAN_POINT('',(0.95,-3.67394039744206E-17,5.7));
#7691=CARTESIAN_POINT('',(0.95,-3.67394039744206E-17,5.7));
#7692=CARTESIAN_POINT('Origin',(1.25,0.,5.7));
#7693=CARTESIAN_POINT('Origin',(1.25,0.,8.95));
#7694=CARTESIAN_POINT('Origin',(1.25,0.,5.7));
#7695=CARTESIAN_POINT('',(0.,0.,0.));
#7696=CARTESIAN_POINT('Origin',(3.75,0.,5.7));
#7697=CARTESIAN_POINT('',(3.55,-2.44929359829471E-17,8.95));
#7698=CARTESIAN_POINT('Origin',(3.75,0.,8.95));
#7699=CARTESIAN_POINT('',(3.55,-2.44929359829471E-17,5.7));
#7700=CARTESIAN_POINT('',(3.55,-2.44929359829471E-17,5.7));
#7701=CARTESIAN_POINT('Origin',(3.75,0.,5.7));
#7702=CARTESIAN_POINT('Origin',(3.75,0.,5.7));
#7703=CARTESIAN_POINT('',(3.45,-3.67394039744206E-17,8.95));
#7704=CARTESIAN_POINT('Origin',(3.75,0.,8.95));
#7705=CARTESIAN_POINT('',(3.45,-3.67394039744206E-17,5.7));
#7706=CARTESIAN_POINT('',(3.45,-3.67394039744206E-17,5.7));
#7707=CARTESIAN_POINT('Origin',(3.75,0.,5.7));
#7708=CARTESIAN_POINT('Origin',(3.75,0.,8.95));
#7709=CARTESIAN_POINT('Origin',(3.75,0.,5.7));
#7710=CARTESIAN_POINT('',(0.,0.,0.));
#7711=CARTESIAN_POINT('Origin',(5.5,0.,3.5));
#7712=CARTESIAN_POINT('',(5.5,0.505181485540923,2.625));
#7713=CARTESIAN_POINT('',(5.5,1.01036297108185,3.5));
#7714=CARTESIAN_POINT('',(5.5,0.505181485540923,2.625));
#7715=CARTESIAN_POINT('',(5.5,-0.505181485540923,2.625));
#7716=CARTESIAN_POINT('',(5.5,-0.505181485540923,2.625));
#7717=CARTESIAN_POINT('',(5.5,-1.01036297108185,3.5));
#7718=CARTESIAN_POINT('',(5.5,-1.01036297108185,3.5));
#7719=CARTESIAN_POINT('',(5.5,-0.505181485540922,4.375));
#7720=CARTESIAN_POINT('',(5.5,-0.505181485540922,4.375));
#7721=CARTESIAN_POINT('',(5.5,0.505181485540923,4.375));
#7722=CARTESIAN_POINT('',(5.5,0.505181485540923,4.375));
#7723=CARTESIAN_POINT('',(5.5,1.01036297108185,3.5));
#7724=CARTESIAN_POINT('',(5.5,-8.38883057415937E-17,4.185));
#7725=CARTESIAN_POINT('Origin',(5.5,0.,3.5));
#7726=CARTESIAN_POINT('Origin',(5.5,-0.505181485540923,2.625));
#7727=CARTESIAN_POINT('',(6.1,0.505181485540923,2.625));
#7728=CARTESIAN_POINT('',(5.5,0.505181485540923,2.625));
#7729=CARTESIAN_POINT('',(6.1,-0.505181485540923,2.625));
#7730=CARTESIAN_POINT('',(6.1,-0.505181485540923,2.625));
#7731=CARTESIAN_POINT('',(5.5,-0.505181485540923,2.625));
#7732=CARTESIAN_POINT('Origin',(5.5,-1.01036297108185,3.5));
#7733=CARTESIAN_POINT('',(6.1,-1.01036297108185,3.5));
#7734=CARTESIAN_POINT('',(6.1,-1.01036297108185,3.5));
#7735=CARTESIAN_POINT('',(5.5,-1.01036297108185,3.5));
#7736=CARTESIAN_POINT('Origin',(5.5,-0.505181485540922,4.375));
#7737=CARTESIAN_POINT('',(6.1,-0.505181485540922,4.375));
#7738=CARTESIAN_POINT('',(6.1,-0.505181485540922,4.375));
#7739=CARTESIAN_POINT('',(5.5,-0.505181485540922,4.375));
#7740=CARTESIAN_POINT('Origin',(5.5,0.505181485540923,4.375));
#7741=CARTESIAN_POINT('',(6.1,0.505181485540923,4.375));
#7742=CARTESIAN_POINT('',(6.1,0.505181485540923,4.375));
#7743=CARTESIAN_POINT('',(5.5,0.505181485540923,4.375));
#7744=CARTESIAN_POINT('Origin',(5.5,1.01036297108185,3.5));
#7745=CARTESIAN_POINT('',(6.1,1.01036297108185,3.5));
#7746=CARTESIAN_POINT('',(6.1,1.01036297108185,3.5));
#7747=CARTESIAN_POINT('',(5.5,1.01036297108185,3.5));
#7748=CARTESIAN_POINT('Origin',(5.5,0.505181485540923,2.625));
#7749=CARTESIAN_POINT('',(6.1,0.505181485540923,2.625));
#7750=CARTESIAN_POINT('Origin',(6.1,0.,3.5));
#7751=CARTESIAN_POINT('Origin',(4.1,0.,3.5));
#7752=CARTESIAN_POINT('',(4.1,-8.38883057415937E-17,4.185));
#7753=CARTESIAN_POINT('',(4.1,-8.38883057415937E-17,4.185));
#7754=CARTESIAN_POINT('Origin',(4.1,0.,3.5));
#7755=CARTESIAN_POINT('Origin',(4.1,0.,3.5));
#7756=CARTESIAN_POINT('',(0.,0.,0.));
#7757=CARTESIAN_POINT('Origin',(-5.,0.,1.6));
#7758=CARTESIAN_POINT('',(-5.15,-1.83697019872103E-17,2.3));
#7759=CARTESIAN_POINT('Origin',(-5.,0.,2.3));
#7760=CARTESIAN_POINT('',(-5.15,-1.83697019872103E-17,1.6));
#7761=CARTESIAN_POINT('',(-5.15,-1.83697019872103E-17,1.6));
#7762=CARTESIAN_POINT('Origin',(-5.,0.,1.6));
#7763=CARTESIAN_POINT('Origin',(-5.,0.,2.3));
#7764=CARTESIAN_POINT('Origin',(-5.,0.,1.6));
#7765=CARTESIAN_POINT('',(0.,0.,0.));
#7766=CARTESIAN_POINT('Origin',(5.,0.,1.6));
#7767=CARTESIAN_POINT('',(4.85,-1.83697019872103E-17,2.3));
#7768=CARTESIAN_POINT('Origin',(5.,0.,2.3));
#7769=CARTESIAN_POINT('',(4.85,-1.83697019872103E-17,1.6));
#7770=CARTESIAN_POINT('',(4.85,-1.83697019872103E-17,1.6));
#7771=CARTESIAN_POINT('Origin',(5.,0.,1.6));
#7772=CARTESIAN_POINT('Origin',(5.,0.,2.3));
#7773=CARTESIAN_POINT('Origin',(5.,0.,1.6));
#7774=CARTESIAN_POINT('',(0.,0.,0.));
#7775=CARTESIAN_POINT('Origin',(-4.5,-2.,4.));
#7776=CARTESIAN_POINT('',(-4.725,-1.95,4.));
#7777=CARTESIAN_POINT('Origin',(-4.5,-1.95,4.));
#7778=CARTESIAN_POINT('',(-4.725,-1.75,4.));
#7779=CARTESIAN_POINT('',(-4.725,-2.,4.));
#7780=CARTESIAN_POINT('Origin',(-4.5,-1.75,4.));
#7781=CARTESIAN_POINT('Origin',(4.5,-2.,4.));
#7782=CARTESIAN_POINT('',(4.275,-1.95,4.));
#7783=CARTESIAN_POINT('Origin',(4.5,-1.95,4.));
#7784=CARTESIAN_POINT('',(4.275,-1.75,4.));
#7785=CARTESIAN_POINT('',(4.275,-2.,4.));
#7786=CARTESIAN_POINT('Origin',(4.5,-1.75,4.));
#7787=CARTESIAN_POINT('Origin',(5.2,-1.75,3.6));
#7788=CARTESIAN_POINT('',(5.2,-1.75,3.6));
#7789=CARTESIAN_POINT('',(-5.2,-1.75,3.6));
#7790=CARTESIAN_POINT('',(5.2,-1.75,3.6));
#7791=CARTESIAN_POINT('',(-5.2,-1.75,4.4));
#7792=CARTESIAN_POINT('',(-5.2,-1.75,3.6));
#7793=CARTESIAN_POINT('',(5.2,-1.75,4.4));
#7794=CARTESIAN_POINT('',(5.2,-1.75,4.4));
#7795=CARTESIAN_POINT('',(5.2,-1.75,3.6));
#7796=CARTESIAN_POINT('Origin',(5.2,-1.95,3.6));
#7797=CARTESIAN_POINT('',(5.2,-1.95,3.6));
#7798=CARTESIAN_POINT('',(5.2,-1.95,3.6));
#7799=CARTESIAN_POINT('',(5.2,-1.95,4.4));
#7800=CARTESIAN_POINT('',(5.2,-1.95,4.4));
#7801=CARTESIAN_POINT('',(5.2,-1.95,3.6));
#7802=CARTESIAN_POINT('Origin',(-5.2,-1.95,3.6));
#7803=CARTESIAN_POINT('',(-5.2,-1.95,3.6));
#7804=CARTESIAN_POINT('',(-5.2,-1.95,3.6));
#7805=CARTESIAN_POINT('',(-5.2,-1.95,4.4));
#7806=CARTESIAN_POINT('',(-5.2,-1.95,4.4));
#7807=CARTESIAN_POINT('',(-5.2,-1.95,3.6));
#7808=CARTESIAN_POINT('Origin',(-5.2,-1.75,3.6));
#7809=CARTESIAN_POINT('',(-5.2,-1.75,3.6));
#7810=CARTESIAN_POINT('',(-5.2,-1.75,4.4));
#7811=CARTESIAN_POINT('Origin',(0.,-1.85,4.4));
#7812=CARTESIAN_POINT('Origin',(0.,-1.85,3.6));
#7813=CARTESIAN_POINT('',(0.,0.,0.));
#7814=CARTESIAN_POINT('Origin',(0.115470053837925,-0.5,-0.2));
#7815=CARTESIAN_POINT('',(0.23094010767585,-0.5,0.));
#7816=CARTESIAN_POINT('',(0.115470053837925,-0.5,-0.2));
#7817=CARTESIAN_POINT('',(0.23094010767585,-0.5,0.));
#7818=CARTESIAN_POINT('',(0.115470053837925,-0.8,-0.2));
#7819=CARTESIAN_POINT('',(0.115470053837925,-0.5,-0.2));
#7820=CARTESIAN_POINT('',(0.23094010767585,-0.8,0.));
#7821=CARTESIAN_POINT('',(0.23094010767585,-0.8,0.));
#7822=CARTESIAN_POINT('',(0.23094010767585,-0.5,0.));
#7823=CARTESIAN_POINT('Origin',(-0.115470053837925,-0.5,-0.2));
#7824=CARTESIAN_POINT('',(-0.115470053837925,-0.5,-0.2));
#7825=CARTESIAN_POINT('',(0.115470053837925,-0.5,-0.2));
#7826=CARTESIAN_POINT('',(-0.115470053837925,-0.8,-0.2));
#7827=CARTESIAN_POINT('',(-0.115470053837925,-0.5,-0.2));
#7828=CARTESIAN_POINT('',(0.115470053837925,-0.8,-0.2));
#7829=CARTESIAN_POINT('Origin',(-0.23094010767585,-0.5,-2.77555756156289E-17));
#7830=CARTESIAN_POINT('',(-0.23094010767585,-0.5,-2.82820063659975E-17));
#7831=CARTESIAN_POINT('',(-0.115470053837925,-0.5,-0.2));
#7832=CARTESIAN_POINT('',(-0.23094010767585,-0.8,-2.77555756156289E-17));
#7833=CARTESIAN_POINT('',(-0.23094010767585,-0.5,-2.82820063659975E-17));
#7834=CARTESIAN_POINT('',(-0.115470053837925,-0.8,-0.2));
#7835=CARTESIAN_POINT('Origin',(-0.115470053837925,-0.5,0.2));
#7836=CARTESIAN_POINT('',(-0.115470053837925,-0.5,0.2));
#7837=CARTESIAN_POINT('',(-0.23094010767585,-0.5,-2.82820063659975E-17));
#7838=CARTESIAN_POINT('',(-0.115470053837925,-0.8,0.2));
#7839=CARTESIAN_POINT('',(-0.115470053837925,-0.5,0.2));
#7840=CARTESIAN_POINT('',(-0.23094010767585,-0.8,-2.82820063659975E-17));
#7841=CARTESIAN_POINT('Origin',(0.115470053837925,-0.5,0.2));
#7842=CARTESIAN_POINT('',(0.115470053837925,-0.5,0.2));
#7843=CARTESIAN_POINT('',(-0.115470053837925,-0.5,0.2));
#7844=CARTESIAN_POINT('',(0.115470053837925,-0.8,0.2));
#7845=CARTESIAN_POINT('',(0.115470053837925,-0.5,0.2));
#7846=CARTESIAN_POINT('',(-0.115470053837925,-0.8,0.2));
#7847=CARTESIAN_POINT('Origin',(0.23094010767585,-0.5,0.));
#7848=CARTESIAN_POINT('',(0.115470053837925,-0.5,0.2));
#7849=CARTESIAN_POINT('',(0.115470053837925,-0.8,0.2));
#7850=CARTESIAN_POINT('Origin',(0.,-0.5,0.));
#7851=CARTESIAN_POINT('Origin',(0.,-0.8,0.));
#7852=CARTESIAN_POINT('Origin',(0.,-1.4,0.));
#7853=CARTESIAN_POINT('',(-0.24505,-1.4,3.00099698131059E-17));
#7854=CARTESIAN_POINT('Origin',(0.,-1.4,0.));
#7855=CARTESIAN_POINT('Origin',(0.375,0.5,0.));
#7856=CARTESIAN_POINT('',(-0.375,0.5,-4.59242549680257E-17));
#7857=CARTESIAN_POINT('Origin',(0.,0.5,0.));
#7858=CARTESIAN_POINT('Origin',(0.,0.475,0.));
#7859=CARTESIAN_POINT('',(-0.425,0.45,-5.20474889637625E-17));
#7860=CARTESIAN_POINT('Origin',(0.,0.45,0.));
#7861=CARTESIAN_POINT('',(-0.4,0.475,-4.89858719658941E-17));
#7862=CARTESIAN_POINT('Origin',(0.,0.24,0.));
#7863=CARTESIAN_POINT('',(-0.425,0.0299999999999998,-5.20474889637625E-17));
#7864=CARTESIAN_POINT('Origin',(0.,0.0299999999999998,0.));
#7865=CARTESIAN_POINT('',(-0.425,0.24,-5.20474889637625E-17));
#7866=CARTESIAN_POINT('Origin',(0.,0.0150000000000001,0.));
#7867=CARTESIAN_POINT('',(-0.395,4.85722573273506E-17,-4.83735485663204E-17));
#7868=CARTESIAN_POINT('Origin',(0.,0.,0.));
#7869=CARTESIAN_POINT('',(-0.41,0.0150000000000001,-5.02105187650415E-17));
#7870=CARTESIAN_POINT('Origin',(0.27,0.,0.));
#7871=CARTESIAN_POINT('',(-0.27,0.,-3.30654635769785E-17));
#7872=CARTESIAN_POINT('Origin',(0.,0.,0.));
#7873=CARTESIAN_POINT('Origin',(0.,-0.02,0.));
#7874=CARTESIAN_POINT('',(-0.24505,-0.0498999999999999,3.00099698131059E-17));
#7875=CARTESIAN_POINT('Origin',(0.,-0.0498999999999999,0.));
#7876=CARTESIAN_POINT('',(-0.26,-0.02,-3.18408167778312E-17));
#7877=CARTESIAN_POINT('Origin',(0.,-0.995,0.));
#7878=CARTESIAN_POINT('',(-0.24505,-0.995,-3.00099698131059E-17));
#7879=CARTESIAN_POINT('',(0.,0.,0.));
#7880=CARTESIAN_POINT('',(0.,0.,0.));
#7881=CARTESIAN_POINT('Origin',(0.,0.6,0.));
#7882=CARTESIAN_POINT('',(-0.43,0.6,5.26598123633362E-17));
#7883=CARTESIAN_POINT('Origin',(0.,0.6,0.));
#7884=CARTESIAN_POINT('',(-0.43,0.7,-5.26598123633362E-17));
#7885=CARTESIAN_POINT('',(-0.43,0.6,5.26598123633362E-17));
#7886=CARTESIAN_POINT('Origin',(0.,0.7,0.));
#7887=CARTESIAN_POINT('Origin',(0.,0.6,0.));
#7888=CARTESIAN_POINT('',(-0.2,0.6,2.44929359829471E-17));
#7889=CARTESIAN_POINT('Origin',(0.,0.6,0.));
#7890=CARTESIAN_POINT('Origin',(0.,0.5,-1.11022302462516E-16));
#7891=CARTESIAN_POINT('',(0.346410161513776,0.5,0.6));
#7892=CARTESIAN_POINT('',(0.692820323027551,0.5,0.));
#7893=CARTESIAN_POINT('',(0.346410161513776,0.5,0.6));
#7894=CARTESIAN_POINT('',(0.346410161513776,0.5,-0.6));
#7895=CARTESIAN_POINT('',(0.692820323027551,0.5,0.));
#7896=CARTESIAN_POINT('',(-0.346410161513775,0.5,-0.6));
#7897=CARTESIAN_POINT('',(0.346410161513776,0.5,-0.6));
#7898=CARTESIAN_POINT('',(-0.692820323027551,0.5,-8.48460190979926E-17));
#7899=CARTESIAN_POINT('',(-0.346410161513775,0.5,-0.6));
#7900=CARTESIAN_POINT('',(-0.346410161513776,0.5,0.6));
#7901=CARTESIAN_POINT('',(-0.692820323027551,0.5,-8.48460190979926E-17));
#7902=CARTESIAN_POINT('',(-0.346410161513776,0.5,0.6));
#7903=CARTESIAN_POINT('',(-0.525,0.5,-6.4293956955236E-17));
#7904=CARTESIAN_POINT('Origin',(0.,0.5,0.));
#7905=CARTESIAN_POINT('Origin',(0.,0.,-1.11022302462516E-16));
#7906=CARTESIAN_POINT('',(0.346410161513776,0.,0.6));
#7907=CARTESIAN_POINT('',(0.692820323027551,0.,0.));
#7908=CARTESIAN_POINT('',(0.346410161513776,0.,0.6));
#7909=CARTESIAN_POINT('',(-0.346410161513776,0.,0.6));
#7910=CARTESIAN_POINT('',(-0.346410161513776,0.,0.6));
#7911=CARTESIAN_POINT('',(-0.692820323027551,0.,-8.48460190979926E-17));
#7912=CARTESIAN_POINT('',(-0.692820323027551,0.,-8.48460190979926E-17));
#7913=CARTESIAN_POINT('',(-0.346410161513775,0.,-0.6));
#7914=CARTESIAN_POINT('',(-0.346410161513775,0.,-0.6));
#7915=CARTESIAN_POINT('',(0.346410161513776,0.,-0.6));
#7916=CARTESIAN_POINT('',(0.346410161513776,0.,-0.6));
#7917=CARTESIAN_POINT('',(0.692820323027551,0.,0.));
#7918=CARTESIAN_POINT('',(-0.515,0.,-6.30693101560887E-17));
#7919=CARTESIAN_POINT('Origin',(0.,0.,0.));
#7920=CARTESIAN_POINT('Origin',(-0.346410161513776,0.,0.6));
#7921=CARTESIAN_POINT('',(0.346410161513776,0.,0.6));
#7922=CARTESIAN_POINT('',(-0.346410161513776,0.,0.6));
#7923=CARTESIAN_POINT('Origin',(-0.692820323027551,0.,-8.48460190979926E-17));
#7924=CARTESIAN_POINT('',(-0.692820323027551,0.,-8.48460190979926E-17));
#7925=CARTESIAN_POINT('Origin',(-0.346410161513775,0.,-0.6));
#7926=CARTESIAN_POINT('',(-0.346410161513775,0.,-0.6));
#7927=CARTESIAN_POINT('Origin',(0.346410161513776,0.,-0.6));
#7928=CARTESIAN_POINT('',(0.346410161513776,0.,-0.6));
#7929=CARTESIAN_POINT('Origin',(0.692820323027551,0.,0.));
#7930=CARTESIAN_POINT('',(0.692820323027551,0.,0.));
#7931=CARTESIAN_POINT('Origin',(0.346410161513776,0.,0.6));
#7932=CARTESIAN_POINT('Origin',(0.46,0.7,0.));
#7933=CARTESIAN_POINT('',(-0.46,0.7,-5.63337527607782E-17));
#7934=CARTESIAN_POINT('Origin',(0.,0.7,0.));
#7935=CARTESIAN_POINT('Origin',(0.,1.2,0.));
#7936=CARTESIAN_POINT('',(-0.46,1.7,-5.63337527607782E-17));
#7937=CARTESIAN_POINT('',(-0.46,1.2,-5.63337527607782E-17));
#7938=CARTESIAN_POINT('Origin',(0.,1.7,0.));
#7939=CARTESIAN_POINT('Origin',(0.525,1.7,0.));
#7940=CARTESIAN_POINT('',(-0.525,1.7,-6.4293956955236E-17));
#7941=CARTESIAN_POINT('Origin',(0.,1.7,0.));
#7942=CARTESIAN_POINT('Origin',(0.,1.1,0.));
#7943=CARTESIAN_POINT('',(-0.525,1.1,-6.4293956955236E-17));
#7944=CARTESIAN_POINT('Origin',(0.,-0.325,0.));
#7945=CARTESIAN_POINT('',(-0.515,-0.65,-6.30693101560887E-17));
#7946=CARTESIAN_POINT('Origin',(0.,-0.65,0.));
#7947=CARTESIAN_POINT('',(-0.515,-0.325,-6.30693101560887E-17));
#7948=CARTESIAN_POINT('Origin',(0.2,-0.65,0.));
#7949=CARTESIAN_POINT('',(-0.2,-0.65,-2.44929359829471E-17));
#7950=CARTESIAN_POINT('Origin',(0.,-0.65,0.));
#7951=CARTESIAN_POINT('Origin',(0.,0.0249999999999999,0.));
#7952=CARTESIAN_POINT('',(-0.2,0.0249999999999999,-2.44929359829471E-17));
#7953=CARTESIAN_POINT('',(0.,0.,0.));
#7954=CARTESIAN_POINT('Origin',(0.475,1.95,0.));
#7955=CARTESIAN_POINT('',(-0.475,1.95,-5.81707229594993E-17));
#7956=CARTESIAN_POINT('Origin',(0.,1.95,0.));
#7957=CARTESIAN_POINT('',(-0.31,1.95,-3.7964050773568E-17));
#7958=CARTESIAN_POINT('Origin',(0.,1.95,0.));
#7959=CARTESIAN_POINT('Origin',(0.,1.825,0.));
#7960=CARTESIAN_POINT('',(-0.475,1.7,-5.81707229594993E-17));
#7961=CARTESIAN_POINT('Origin',(0.,1.7,0.));
#7962=CARTESIAN_POINT('',(-0.475,1.825,-5.81707229594993E-17));
#7963=CARTESIAN_POINT('Origin',(0.355,1.7,0.));
#7964=CARTESIAN_POINT('',(-0.355,1.7,-4.3474961369731E-17));
#7965=CARTESIAN_POINT('Origin',(0.,1.7,0.));
#7966=CARTESIAN_POINT('Origin',(0.,1.55,0.));
#7967=CARTESIAN_POINT('',(-0.355,1.4,-4.3474961369731E-17));
#7968=CARTESIAN_POINT('Origin',(0.,1.4,0.));
#7969=CARTESIAN_POINT('',(-0.355,1.55,-4.3474961369731E-17));
#7970=CARTESIAN_POINT('Origin',(0.31,1.4,0.));
#7971=CARTESIAN_POINT('',(-0.31,1.4,-3.7964050773568E-17));
#7972=CARTESIAN_POINT('Origin',(0.,1.4,0.));
#7973=CARTESIAN_POINT('Origin',(0.,1.675,0.));
#7974=CARTESIAN_POINT('',(-0.31,1.675,-3.7964050773568E-17));
#7975=CARTESIAN_POINT('',(0.,0.,0.));
#7976=CARTESIAN_POINT('',(0.,0.,0.));
#7977=CARTESIAN_POINT('',(0.,0.,0.));
#7978=CARTESIAN_POINT('Origin',(0.,-0.4,0.));
#7979=CARTESIAN_POINT('',(1.01036297108185,-0.4,0.));
#7980=CARTESIAN_POINT('',(0.505181485540923,-0.4,0.875));
#7981=CARTESIAN_POINT('',(0.505181485540923,-0.4,0.875));
#7982=CARTESIAN_POINT('',(-0.505181485540923,-0.4,0.875));
#7983=CARTESIAN_POINT('',(-0.505181485540923,-0.4,0.875));
#7984=CARTESIAN_POINT('',(-1.01036297108185,-0.4,-1.23733777851239E-16));
#7985=CARTESIAN_POINT('',(-1.01036297108185,-0.4,-1.23733777851239E-16));
#7986=CARTESIAN_POINT('',(-0.505181485540922,-0.4,-0.875));
#7987=CARTESIAN_POINT('',(-0.505181485540922,-0.4,-0.875));
#7988=CARTESIAN_POINT('',(0.505181485540923,-0.4,-0.875));
#7989=CARTESIAN_POINT('',(0.505181485540923,-0.4,-0.875));
#7990=CARTESIAN_POINT('',(1.01036297108185,-0.4,0.));
#7991=CARTESIAN_POINT('',(-0.685,-0.4,-8.38883057415937E-17));
#7992=CARTESIAN_POINT('Origin',(0.,-0.4,0.));
#7993=CARTESIAN_POINT('Origin',(0.,0.4,0.));
#7994=CARTESIAN_POINT('',(0.505181485540923,0.4,0.875));
#7995=CARTESIAN_POINT('',(1.01036297108185,0.4,0.));
#7996=CARTESIAN_POINT('',(0.505181485540923,0.4,0.875));
#7997=CARTESIAN_POINT('',(0.505181485540923,0.4,-0.875));
#7998=CARTESIAN_POINT('',(1.01036297108185,0.4,0.));
#7999=CARTESIAN_POINT('',(-0.505181485540922,0.4,-0.875));
#8000=CARTESIAN_POINT('',(0.505181485540923,0.4,-0.875));
#8001=CARTESIAN_POINT('',(-1.01036297108185,0.4,-1.23733777851239E-16));
#8002=CARTESIAN_POINT('',(-0.505181485540922,0.4,-0.875));
#8003=CARTESIAN_POINT('',(-0.505181485540923,0.4,0.875));
#8004=CARTESIAN_POINT('',(-1.01036297108185,0.4,-1.23733777851239E-16));
#8005=CARTESIAN_POINT('',(-0.505181485540923,0.4,0.875));
#8006=CARTESIAN_POINT('',(-0.685,0.4,8.38883057415937E-17));
#8007=CARTESIAN_POINT('Origin',(0.,0.4,0.));
#8008=CARTESIAN_POINT('Origin',(-0.505181485540923,0.,0.875));
#8009=CARTESIAN_POINT('',(0.505181485540923,0.,0.875));
#8010=CARTESIAN_POINT('',(-0.505181485540923,0.,0.875));
#8011=CARTESIAN_POINT('Origin',(-1.01036297108185,0.,-1.23733777851239E-16));
#8012=CARTESIAN_POINT('',(-1.01036297108185,0.,-1.23733777851239E-16));
#8013=CARTESIAN_POINT('Origin',(-0.505181485540922,0.,-0.875));
#8014=CARTESIAN_POINT('',(-0.505181485540922,0.,-0.875));
#8015=CARTESIAN_POINT('Origin',(0.505181485540923,0.,-0.875));
#8016=CARTESIAN_POINT('',(0.505181485540923,0.,-0.875));
#8017=CARTESIAN_POINT('Origin',(1.01036297108185,0.,0.));
#8018=CARTESIAN_POINT('',(1.01036297108185,0.,0.));
#8019=CARTESIAN_POINT('Origin',(0.505181485540923,0.,0.875));
#8020=CARTESIAN_POINT('Origin',(0.,0.,0.));
#8021=CARTESIAN_POINT('',(-0.685,1.82,-8.38883057415937E-17));
#8022=CARTESIAN_POINT('',(-0.685,0.,-8.38883057415937E-17));
#8023=CARTESIAN_POINT('Origin',(0.,1.82,0.));
#8024=CARTESIAN_POINT('Origin',(0.605,1.9,0.));
#8025=CARTESIAN_POINT('',(-0.605,1.9,-7.40911313484149E-17));
#8026=CARTESIAN_POINT('Origin',(0.,1.9,0.));
#8027=CARTESIAN_POINT('',(-0.46,1.9,-5.63337527607782E-17));
#8028=CARTESIAN_POINT('Origin',(0.,1.9,0.));
#8029=CARTESIAN_POINT('Origin',(0.,1.86,0.));
#8030=CARTESIAN_POINT('',(-0.645,1.86,-7.89897185450043E-17));
#8031=CARTESIAN_POINT('Origin',(0.,0.,0.));
#8032=CARTESIAN_POINT('',(-0.685,-1.82,-8.38883057415937E-17));
#8033=CARTESIAN_POINT('Origin',(0.,-1.82,0.));
#8034=CARTESIAN_POINT('',(-0.685,0.,-8.38883057415937E-17));
#8035=CARTESIAN_POINT('Origin',(0.,-1.86,0.));
#8036=CARTESIAN_POINT('',(-0.605,-1.9,-7.40911313484149E-17));
#8037=CARTESIAN_POINT('Origin',(0.,-1.9,0.));
#8038=CARTESIAN_POINT('',(-0.645,-1.86,-7.89897185450043E-17));
#8039=CARTESIAN_POINT('Origin',(0.46,-1.9,0.));
#8040=CARTESIAN_POINT('',(-0.46,-1.9,-5.63337527607782E-17));
#8041=CARTESIAN_POINT('Origin',(0.,-1.9,0.));
#8042=CARTESIAN_POINT('Origin',(0.,0.,0.));
#8043=CARTESIAN_POINT('',(-0.46,0.,-5.63337527607782E-17));
#8044=CARTESIAN_POINT('',(0.,0.,0.));
#8045=CARTESIAN_POINT('Origin',(0.3,0.4,0.));
#8046=CARTESIAN_POINT('',(-0.3,0.4,-3.67394039744206E-17));
#8047=CARTESIAN_POINT('Origin',(0.,0.4,0.));
#8048=CARTESIAN_POINT('Origin',(0.,0.375,0.));
#8049=CARTESIAN_POINT('',(-0.35,0.35,-4.28626379701573E-17));
#8050=CARTESIAN_POINT('Origin',(0.,0.35,0.));
#8051=CARTESIAN_POINT('',(-0.325,0.375,-3.9801020972289E-17));
#8052=CARTESIAN_POINT('Origin',(0.,0.19,0.));
#8053=CARTESIAN_POINT('',(-0.35,0.03,-4.28626379701574E-17));
#8054=CARTESIAN_POINT('Origin',(0.,0.03,0.));
#8055=CARTESIAN_POINT('',(-0.35,0.19,-4.28626379701574E-17));
#8056=CARTESIAN_POINT('Origin',(0.,0.0149999999999999,0.));
#8057=CARTESIAN_POINT('',(-0.32,-3.29597460435593E-17,-3.91886975727153E-17));
#8058=CARTESIAN_POINT('Origin',(0.,0.,0.));
#8059=CARTESIAN_POINT('',(-0.335,0.0149999999999999,-4.10256677714363E-17));
#8060=CARTESIAN_POINT('Origin',(0.22,0.,0.));
#8061=CARTESIAN_POINT('',(-0.22,-6.93889390390723E-18,-2.69422295812418E-17));
#8062=CARTESIAN_POINT('Origin',(0.,0.,0.));
#8063=CARTESIAN_POINT('Origin',(0.,-0.02,0.));
#8064=CARTESIAN_POINT('',(-0.1954,-0.0492,2.39295984553393E-17));
#8065=CARTESIAN_POINT('Origin',(0.,-0.0492,0.));
#8066=CARTESIAN_POINT('',(-0.21,-0.02,-2.57175827820944E-17));
#8067=CARTESIAN_POINT('Origin',(0.,-0.8,0.));
#8068=CARTESIAN_POINT('',(-0.1954,-1.5646,2.39295984553393E-17));
#8069=CARTESIAN_POINT('Origin',(0.,-1.5646,0.));
#8070=CARTESIAN_POINT('',(-0.1954,-0.8,-2.39295984553393E-17));
#8071=CARTESIAN_POINT('Origin',(0.,-1.58,0.));
#8072=CARTESIAN_POINT('',(-0.16,-1.6,-1.95943487863577E-17));
#8073=CARTESIAN_POINT('Origin',(0.,-1.6,0.));
#8074=CARTESIAN_POINT('',(-0.18,-1.58,-2.20436423846524E-17));
#8075=CARTESIAN_POINT('Origin',(0.,-1.6,0.));
#8076=CARTESIAN_POINT('Origin',(0.0866025403784439,-0.4,-0.15));
#8077=CARTESIAN_POINT('',(0.173205080756888,-0.4,0.));
#8078=CARTESIAN_POINT('',(0.0866025403784439,-0.4,-0.15));
#8079=CARTESIAN_POINT('',(0.173205080756888,-0.4,0.));
#8080=CARTESIAN_POINT('',(0.0866025403784439,-0.64,-0.15));
#8081=CARTESIAN_POINT('',(0.0866025403784439,-0.4,-0.15));
#8082=CARTESIAN_POINT('',(0.173205080756888,-0.64,0.));
#8083=CARTESIAN_POINT('',(0.173205080756888,-0.64,0.));
#8084=CARTESIAN_POINT('',(0.173205080756888,-0.4,0.));
#8085=CARTESIAN_POINT('Origin',(-0.0866025403784438,-0.4,-0.15));
#8086=CARTESIAN_POINT('',(-0.0866025403784438,-0.4,-0.15));
#8087=CARTESIAN_POINT('',(0.0866025403784439,-0.4,-0.15));
#8088=CARTESIAN_POINT('',(-0.0866025403784438,-0.64,-0.15));
#8089=CARTESIAN_POINT('',(-0.0866025403784438,-0.4,-0.15));
#8090=CARTESIAN_POINT('',(0.0866025403784439,-0.64,-0.15));
#8091=CARTESIAN_POINT('Origin',(-0.173205080756888,-0.4,-2.77555756156289E-17));
#8092=CARTESIAN_POINT('',(-0.173205080756888,-0.4,-2.12115047744981E-17));
#8093=CARTESIAN_POINT('',(-0.0866025403784438,-0.4,-0.15));
#8094=CARTESIAN_POINT('',(-0.173205080756888,-0.64,-2.77555756156289E-17));
#8095=CARTESIAN_POINT('',(-0.173205080756888,-0.4,-2.12115047744981E-17));
#8096=CARTESIAN_POINT('',(-0.0866025403784438,-0.64,-0.15));
#8097=CARTESIAN_POINT('Origin',(-0.0866025403784439,-0.4,0.15));
#8098=CARTESIAN_POINT('',(-0.0866025403784439,-0.4,0.15));
#8099=CARTESIAN_POINT('',(-0.173205080756888,-0.4,-2.12115047744981E-17));
#8100=CARTESIAN_POINT('',(-0.0866025403784439,-0.64,0.15));
#8101=CARTESIAN_POINT('',(-0.0866025403784439,-0.4,0.15));
#8102=CARTESIAN_POINT('',(-0.173205080756888,-0.64,-2.12115047744981E-17));
#8103=CARTESIAN_POINT('Origin',(0.0866025403784439,-0.4,0.15));
#8104=CARTESIAN_POINT('',(0.0866025403784439,-0.4,0.15));
#8105=CARTESIAN_POINT('',(-0.0866025403784439,-0.4,0.15));
#8106=CARTESIAN_POINT('',(0.0866025403784439,-0.64,0.15));
#8107=CARTESIAN_POINT('',(0.0866025403784439,-0.4,0.15));
#8108=CARTESIAN_POINT('',(-0.0866025403784439,-0.64,0.15));
#8109=CARTESIAN_POINT('Origin',(0.173205080756888,-0.4,0.));
#8110=CARTESIAN_POINT('',(0.0866025403784439,-0.4,0.15));
#8111=CARTESIAN_POINT('',(0.0866025403784439,-0.64,0.15));
#8112=CARTESIAN_POINT('Origin',(0.,-0.4,-2.77555756156289E-17));
#8113=CARTESIAN_POINT('Origin',(0.,-0.64,-2.77555756156289E-17));
#8114=CARTESIAN_POINT('',(0.,0.,0.));
#8115=CARTESIAN_POINT('Origin',(0.0866025403784439,-0.4,-0.15));
#8116=CARTESIAN_POINT('',(0.173205080756888,-0.4,0.));
#8117=CARTESIAN_POINT('',(0.0866025403784439,-0.4,-0.15));
#8118=CARTESIAN_POINT('',(0.173205080756888,-0.4,0.));
#8119=CARTESIAN_POINT('',(0.0866025403784439,-0.64,-0.15));
#8120=CARTESIAN_POINT('',(0.0866025403784439,-0.4,-0.15));
#8121=CARTESIAN_POINT('',(0.173205080756888,-0.64,0.));
#8122=CARTESIAN_POINT('',(0.173205080756888,-0.64,0.));
#8123=CARTESIAN_POINT('',(0.173205080756888,-0.4,0.));
#8124=CARTESIAN_POINT('Origin',(-0.0866025403784438,-0.4,-0.15));
#8125=CARTESIAN_POINT('',(-0.0866025403784438,-0.4,-0.15));
#8126=CARTESIAN_POINT('',(0.0866025403784439,-0.4,-0.15));
#8127=CARTESIAN_POINT('',(-0.0866025403784438,-0.64,-0.15));
#8128=CARTESIAN_POINT('',(-0.0866025403784438,-0.4,-0.15));
#8129=CARTESIAN_POINT('',(0.0866025403784439,-0.64,-0.15));
#8130=CARTESIAN_POINT('Origin',(-0.173205080756888,-0.4,-2.77555756156289E-17));
#8131=CARTESIAN_POINT('',(-0.173205080756888,-0.4,-2.12115047744981E-17));
#8132=CARTESIAN_POINT('',(-0.0866025403784438,-0.4,-0.15));
#8133=CARTESIAN_POINT('',(-0.173205080756888,-0.64,-2.77555756156289E-17));
#8134=CARTESIAN_POINT('',(-0.173205080756888,-0.4,-2.12115047744981E-17));
#8135=CARTESIAN_POINT('',(-0.0866025403784438,-0.64,-0.15));
#8136=CARTESIAN_POINT('Origin',(-0.0866025403784439,-0.4,0.15));
#8137=CARTESIAN_POINT('',(-0.0866025403784439,-0.4,0.15));
#8138=CARTESIAN_POINT('',(-0.173205080756888,-0.4,-2.12115047744981E-17));
#8139=CARTESIAN_POINT('',(-0.0866025403784439,-0.64,0.15));
#8140=CARTESIAN_POINT('',(-0.0866025403784439,-0.4,0.15));
#8141=CARTESIAN_POINT('',(-0.173205080756888,-0.64,-2.12115047744981E-17));
#8142=CARTESIAN_POINT('Origin',(0.0866025403784439,-0.4,0.15));
#8143=CARTESIAN_POINT('',(0.0866025403784439,-0.4,0.15));
#8144=CARTESIAN_POINT('',(-0.0866025403784439,-0.4,0.15));
#8145=CARTESIAN_POINT('',(0.0866025403784439,-0.64,0.15));
#8146=CARTESIAN_POINT('',(0.0866025403784439,-0.4,0.15));
#8147=CARTESIAN_POINT('',(-0.0866025403784439,-0.64,0.15));
#8148=CARTESIAN_POINT('Origin',(0.173205080756888,-0.4,0.));
#8149=CARTESIAN_POINT('',(0.0866025403784439,-0.4,0.15));
#8150=CARTESIAN_POINT('',(0.0866025403784439,-0.64,0.15));
#8151=CARTESIAN_POINT('Origin',(0.,-0.4,-2.77555756156289E-17));
#8152=CARTESIAN_POINT('Origin',(0.,-0.64,-2.77555756156289E-17));
#8153=CARTESIAN_POINT('Origin',(0.,-1.,0.));
#8154=CARTESIAN_POINT('',(-0.1954,-1.,2.39295984553393E-17));
#8155=CARTESIAN_POINT('Origin',(0.,-1.,0.));
#8156=CARTESIAN_POINT('Origin',(0.3,0.4,0.));
#8157=CARTESIAN_POINT('',(-0.3,0.4,-3.67394039744206E-17));
#8158=CARTESIAN_POINT('Origin',(0.,0.4,0.));
#8159=CARTESIAN_POINT('Origin',(0.,0.375,0.));
#8160=CARTESIAN_POINT('',(-0.35,0.35,-4.28626379701573E-17));
#8161=CARTESIAN_POINT('Origin',(0.,0.35,0.));
#8162=CARTESIAN_POINT('',(-0.325,0.375,-3.9801020972289E-17));
#8163=CARTESIAN_POINT('Origin',(0.,0.19,0.));
#8164=CARTESIAN_POINT('',(-0.35,0.03,-4.28626379701574E-17));
#8165=CARTESIAN_POINT('Origin',(0.,0.03,0.));
#8166=CARTESIAN_POINT('',(-0.35,0.19,-4.28626379701574E-17));
#8167=CARTESIAN_POINT('Origin',(0.,0.0149999999999999,0.));
#8168=CARTESIAN_POINT('',(-0.32,-3.29597460435593E-17,-3.91886975727153E-17));
#8169=CARTESIAN_POINT('Origin',(0.,0.,0.));
#8170=CARTESIAN_POINT('',(-0.335,0.0149999999999999,-4.10256677714363E-17));
#8171=CARTESIAN_POINT('Origin',(0.22,0.,0.));
#8172=CARTESIAN_POINT('',(-0.22,-6.93889390390723E-18,-2.69422295812418E-17));
#8173=CARTESIAN_POINT('Origin',(0.,0.,0.));
#8174=CARTESIAN_POINT('Origin',(0.,-0.02,0.));
#8175=CARTESIAN_POINT('',(-0.1954,-0.0492,2.39295984553393E-17));
#8176=CARTESIAN_POINT('Origin',(0.,-0.0492,0.));
#8177=CARTESIAN_POINT('',(-0.21,-0.02,-2.57175827820944E-17));
#8178=CARTESIAN_POINT('Origin',(0.,-0.8,0.));
#8179=CARTESIAN_POINT('',(-0.1954,-0.8,-2.39295984553393E-17));
#8180=CARTESIAN_POINT('',(0.,0.,0.));
#8181=CARTESIAN_POINT('',(0.,0.,0.));
#8182=CARTESIAN_POINT('',(0.,0.,0.));
#8183=CARTESIAN_POINT('',(0.,0.,0.));
#8184=CARTESIAN_POINT('',(0.,0.,0.));
#8185=CARTESIAN_POINT('',(0.,0.,0.));
#8186=CARTESIAN_POINT('',(0.,0.,0.));
#8187=CARTESIAN_POINT('',(0.,0.,0.));
#8188=CARTESIAN_POINT('',(0.,0.,0.));
#8189=CARTESIAN_POINT('',(0.,0.,0.));
#8190=CARTESIAN_POINT('',(0.,0.,0.));
#8191=CARTESIAN_POINT('',(0.,0.,0.));
#8192=CARTESIAN_POINT('',(0.,0.,0.));
#8193=CARTESIAN_POINT('',(0.,0.,0.));
#8194=CARTESIAN_POINT('',(0.,0.,0.));
#8195=CARTESIAN_POINT('',(0.,0.,0.));
#8196=CARTESIAN_POINT('',(-5.,-2.8,1.4));
#8197=CARTESIAN_POINT('',(-5.,2.8,1.4));
#8198=CARTESIAN_POINT('',(-5.,-1.8,0.4));
#8199=CARTESIAN_POINT('',(-5.,1.8,0.4));
#8200=CARTESIAN_POINT('',(5.,-2.8,1.4));
#8201=CARTESIAN_POINT('',(5.,2.8,1.4));
#8202=CARTESIAN_POINT('',(5.,-1.8,0.4));
#8203=CARTESIAN_POINT('',(5.,1.8,0.4));
#8204=CARTESIAN_POINT('',(-3.75,0.,5.));
#8205=CARTESIAN_POINT('',(-1.25,0.,5.));
#8206=CARTESIAN_POINT('',(1.25,0.,5.));
#8207=CARTESIAN_POINT('',(3.75,0.,5.));
#8208=CARTESIAN_POINT('',(-6.,0.,3.5));
#8209=CARTESIAN_POINT('',(-4.5,-1.4,1.4));
#8210=CARTESIAN_POINT('',(-4.5,1.4,1.4));
#8211=CARTESIAN_POINT('',(0.,-1.4,1.4));
#8212=CARTESIAN_POINT('',(0.,1.4,1.4));
#8213=CARTESIAN_POINT('',(4.5,-1.4,1.4));
#8214=CARTESIAN_POINT('',(4.5,1.4,1.4));
#8215=CARTESIAN_POINT('',(-4.5,-1.95,4.));
#8216=CARTESIAN_POINT('',(4.5,-1.95,4.));
#8217=UNCERTAINTY_MEASURE_WITH_UNIT(LENGTH_MEASURE(0.001),#8267,
'DISTANCE_ACCURACY_VALUE',
'Maximum model space distance between geometric entities at asserted c
onnectivities');
#8218=UNCERTAINTY_MEASURE_WITH_UNIT(LENGTH_MEASURE(0.001),#8267,
'DISTANCE_ACCURACY_VALUE',
'Maximum model space distance between geometric entities at asserted c
onnectivities');
#8219=UNCERTAINTY_MEASURE_WITH_UNIT(LENGTH_MEASURE(0.001),#8267,
'DISTANCE_ACCURACY_VALUE',
'Maximum model space distance between geometric entities at asserted c
onnectivities');
#8220=UNCERTAINTY_MEASURE_WITH_UNIT(LENGTH_MEASURE(0.001),#8267,
'DISTANCE_ACCURACY_VALUE',
'Maximum model space distance between geometric entities at asserted c
onnectivities');
#8221=UNCERTAINTY_MEASURE_WITH_UNIT(LENGTH_MEASURE(0.001),#8267,
'DISTANCE_ACCURACY_VALUE',
'Maximum model space distance between geometric entities at asserted c
onnectivities');
#8222=UNCERTAINTY_MEASURE_WITH_UNIT(LENGTH_MEASURE(0.001),#8267,
'DISTANCE_ACCURACY_VALUE',
'Maximum model space distance between geometric entities at asserted c
onnectivities');
#8223=UNCERTAINTY_MEASURE_WITH_UNIT(LENGTH_MEASURE(0.001),#8267,
'DISTANCE_ACCURACY_VALUE',
'Maximum model space distance between geometric entities at asserted c
onnectivities');
#8224=UNCERTAINTY_MEASURE_WITH_UNIT(LENGTH_MEASURE(0.001),#8267,
'DISTANCE_ACCURACY_VALUE',
'Maximum model space distance between geometric entities at asserted c
onnectivities');
#8225=UNCERTAINTY_MEASURE_WITH_UNIT(LENGTH_MEASURE(0.001),#8267,
'DISTANCE_ACCURACY_VALUE',
'Maximum model space distance between geometric entities at asserted c
onnectivities');
#8226=UNCERTAINTY_MEASURE_WITH_UNIT(LENGTH_MEASURE(0.001),#8267,
'DISTANCE_ACCURACY_VALUE',
'Maximum model space distance between geometric entities at asserted c
onnectivities');
#8227=UNCERTAINTY_MEASURE_WITH_UNIT(LENGTH_MEASURE(0.001),#8267,
'DISTANCE_ACCURACY_VALUE',
'Maximum model space distance between geometric entities at asserted c
onnectivities');
#8228=UNCERTAINTY_MEASURE_WITH_UNIT(LENGTH_MEASURE(0.001),#8267,
'DISTANCE_ACCURACY_VALUE',
'Maximum model space distance between geometric entities at asserted c
onnectivities');
#8229=UNCERTAINTY_MEASURE_WITH_UNIT(LENGTH_MEASURE(0.001),#8267,
'DISTANCE_ACCURACY_VALUE',
'Maximum model space distance between geometric entities at asserted c
onnectivities');
#8230=UNCERTAINTY_MEASURE_WITH_UNIT(LENGTH_MEASURE(0.001),#8267,
'DISTANCE_ACCURACY_VALUE',
'Maximum model space distance between geometric entities at asserted c
onnectivities');
#8231=UNCERTAINTY_MEASURE_WITH_UNIT(LENGTH_MEASURE(0.001),#8267,
'DISTANCE_ACCURACY_VALUE',
'Maximum model space distance between geometric entities at asserted c
onnectivities');
#8232=UNCERTAINTY_MEASURE_WITH_UNIT(LENGTH_MEASURE(0.001),#8267,
'DISTANCE_ACCURACY_VALUE',
'Maximum model space distance between geometric entities at asserted c
onnectivities');
#8233=UNCERTAINTY_MEASURE_WITH_UNIT(LENGTH_MEASURE(0.001),#8267,
'DISTANCE_ACCURACY_VALUE',
'Maximum model space distance between geometric entities at asserted c
onnectivities');
#8234=UNCERTAINTY_MEASURE_WITH_UNIT(LENGTH_MEASURE(0.001),#8267,
'DISTANCE_ACCURACY_VALUE',
'Maximum model space distance between geometric entities at asserted c
onnectivities');
#8235=UNCERTAINTY_MEASURE_WITH_UNIT(LENGTH_MEASURE(0.001),#8267,
'DISTANCE_ACCURACY_VALUE',
'Maximum model space distance between geometric entities at asserted c
onnectivities');
#8236=UNCERTAINTY_MEASURE_WITH_UNIT(LENGTH_MEASURE(0.001),#8267,
'DISTANCE_ACCURACY_VALUE',
'Maximum model space distance between geometric entities at asserted c
onnectivities');
#8237=UNCERTAINTY_MEASURE_WITH_UNIT(LENGTH_MEASURE(0.001),#8267,
'DISTANCE_ACCURACY_VALUE',
'Maximum model space distance between geometric entities at asserted c
onnectivities');
#8238=UNCERTAINTY_MEASURE_WITH_UNIT(LENGTH_MEASURE(0.001),#8267,
'DISTANCE_ACCURACY_VALUE',
'Maximum model space distance between geometric entities at asserted c
onnectivities');
#8239=UNCERTAINTY_MEASURE_WITH_UNIT(LENGTH_MEASURE(0.001),#8267,
'DISTANCE_ACCURACY_VALUE',
'Maximum model space distance between geometric entities at asserted c
onnectivities');
#8240=UNCERTAINTY_MEASURE_WITH_UNIT(LENGTH_MEASURE(0.001),#8267,
'DISTANCE_ACCURACY_VALUE',
'Maximum model space distance between geometric entities at asserted c
onnectivities');
#8241=UNCERTAINTY_MEASURE_WITH_UNIT(LENGTH_MEASURE(0.001),#8267,
'DISTANCE_ACCURACY_VALUE',
'Maximum model space distance between geometric entities at asserted c
onnectivities');
#8242=(
GEOMETRIC_REPRESENTATION_CONTEXT(3)
GLOBAL_UNCERTAINTY_ASSIGNED_CONTEXT((#8217))
GLOBAL_UNIT_ASSIGNED_CONTEXT((#8267,#8269,#8270))
REPRESENTATION_CONTEXT('','3D')
);
#8243=(
GEOMETRIC_REPRESENTATION_CONTEXT(3)
GLOBAL_UNCERTAINTY_ASSIGNED_CONTEXT((#8218))
GLOBAL_UNIT_ASSIGNED_CONTEXT((#8267,#8269,#8270))
REPRESENTATION_CONTEXT('','3D')
);
#8244=(
GEOMETRIC_REPRESENTATION_CONTEXT(3)
GLOBAL_UNCERTAINTY_ASSIGNED_CONTEXT((#8219))
GLOBAL_UNIT_ASSIGNED_CONTEXT((#8267,#8269,#8270))
REPRESENTATION_CONTEXT('','3D')
);
#8245=(
GEOMETRIC_REPRESENTATION_CONTEXT(3)
GLOBAL_UNCERTAINTY_ASSIGNED_CONTEXT((#8220))
GLOBAL_UNIT_ASSIGNED_CONTEXT((#8267,#8269,#8270))
REPRESENTATION_CONTEXT('','3D')
);
#8246=(
GEOMETRIC_REPRESENTATION_CONTEXT(3)
GLOBAL_UNCERTAINTY_ASSIGNED_CONTEXT((#8221))
GLOBAL_UNIT_ASSIGNED_CONTEXT((#8267,#8269,#8270))
REPRESENTATION_CONTEXT('','3D')
);
#8247=(
GEOMETRIC_REPRESENTATION_CONTEXT(3)
GLOBAL_UNCERTAINTY_ASSIGNED_CONTEXT((#8222))
GLOBAL_UNIT_ASSIGNED_CONTEXT((#8267,#8269,#8270))
REPRESENTATION_CONTEXT('','3D')
);
#8248=(
GEOMETRIC_REPRESENTATION_CONTEXT(3)
GLOBAL_UNCERTAINTY_ASSIGNED_CONTEXT((#8223))
GLOBAL_UNIT_ASSIGNED_CONTEXT((#8267,#8269,#8270))
REPRESENTATION_CONTEXT('','3D')
);
#8249=(
GEOMETRIC_REPRESENTATION_CONTEXT(3)
GLOBAL_UNCERTAINTY_ASSIGNED_CONTEXT((#8224))
GLOBAL_UNIT_ASSIGNED_CONTEXT((#8267,#8269,#8270))
REPRESENTATION_CONTEXT('','3D')
);
#8250=(
GEOMETRIC_REPRESENTATION_CONTEXT(3)
GLOBAL_UNCERTAINTY_ASSIGNED_CONTEXT((#8225))
GLOBAL_UNIT_ASSIGNED_CONTEXT((#8267,#8269,#8270))
REPRESENTATION_CONTEXT('','3D')
);
#8251=(
GEOMETRIC_REPRESENTATION_CONTEXT(3)
GLOBAL_UNCERTAINTY_ASSIGNED_CONTEXT((#8226))
GLOBAL_UNIT_ASSIGNED_CONTEXT((#8267,#8269,#8270))
REPRESENTATION_CONTEXT('','3D')
);
#8252=(
GEOMETRIC_REPRESENTATION_CONTEXT(3)
GLOBAL_UNCERTAINTY_ASSIGNED_CONTEXT((#8227))
GLOBAL_UNIT_ASSIGNED_CONTEXT((#8267,#8269,#8270))
REPRESENTATION_CONTEXT('','3D')
);
#8253=(
GEOMETRIC_REPRESENTATION_CONTEXT(3)
GLOBAL_UNCERTAINTY_ASSIGNED_CONTEXT((#8228))
GLOBAL_UNIT_ASSIGNED_CONTEXT((#8267,#8269,#8270))
REPRESENTATION_CONTEXT('','3D')
);
#8254=(
GEOMETRIC_REPRESENTATION_CONTEXT(3)
GLOBAL_UNCERTAINTY_ASSIGNED_CONTEXT((#8229))
GLOBAL_UNIT_ASSIGNED_CONTEXT((#8267,#8269,#8270))
REPRESENTATION_CONTEXT('','3D')
);
#8255=(
GEOMETRIC_REPRESENTATION_CONTEXT(3)
GLOBAL_UNCERTAINTY_ASSIGNED_CONTEXT((#8230))
GLOBAL_UNIT_ASSIGNED_CONTEXT((#8267,#8269,#8270))
REPRESENTATION_CONTEXT('','3D')
);
#8256=(
GEOMETRIC_REPRESENTATION_CONTEXT(3)
GLOBAL_UNCERTAINTY_ASSIGNED_CONTEXT((#8231))
GLOBAL_UNIT_ASSIGNED_CONTEXT((#8267,#8269,#8270))
REPRESENTATION_CONTEXT('','3D')
);
#8257=(
GEOMETRIC_REPRESENTATION_CONTEXT(3)
GLOBAL_UNCERTAINTY_ASSIGNED_CONTEXT((#8232))
GLOBAL_UNIT_ASSIGNED_CONTEXT((#8267,#8269,#8270))
REPRESENTATION_CONTEXT('','3D')
);
#8258=(
GEOMETRIC_REPRESENTATION_CONTEXT(3)
GLOBAL_UNCERTAINTY_ASSIGNED_CONTEXT((#8233))
GLOBAL_UNIT_ASSIGNED_CONTEXT((#8267,#8269,#8270))
REPRESENTATION_CONTEXT('','3D')
);
#8259=(
GEOMETRIC_REPRESENTATION_CONTEXT(3)
GLOBAL_UNCERTAINTY_ASSIGNED_CONTEXT((#8234))
GLOBAL_UNIT_ASSIGNED_CONTEXT((#8267,#8269,#8270))
REPRESENTATION_CONTEXT('','3D')
);
#8260=(
GEOMETRIC_REPRESENTATION_CONTEXT(3)
GLOBAL_UNCERTAINTY_ASSIGNED_CONTEXT((#8235))
GLOBAL_UNIT_ASSIGNED_CONTEXT((#8267,#8269,#8270))
REPRESENTATION_CONTEXT('','3D')
);
#8261=(
GEOMETRIC_REPRESENTATION_CONTEXT(3)
GLOBAL_UNCERTAINTY_ASSIGNED_CONTEXT((#8236))
GLOBAL_UNIT_ASSIGNED_CONTEXT((#8267,#8269,#8270))
REPRESENTATION_CONTEXT('','3D')
);
#8262=(
GEOMETRIC_REPRESENTATION_CONTEXT(3)
GLOBAL_UNCERTAINTY_ASSIGNED_CONTEXT((#8237))
GLOBAL_UNIT_ASSIGNED_CONTEXT((#8267,#8269,#8270))
REPRESENTATION_CONTEXT('','3D')
);
#8263=(
GEOMETRIC_REPRESENTATION_CONTEXT(3)
GLOBAL_UNCERTAINTY_ASSIGNED_CONTEXT((#8238))
GLOBAL_UNIT_ASSIGNED_CONTEXT((#8267,#8269,#8270))
REPRESENTATION_CONTEXT('','3D')
);
#8264=(
GEOMETRIC_REPRESENTATION_CONTEXT(3)
GLOBAL_UNCERTAINTY_ASSIGNED_CONTEXT((#8239))
GLOBAL_UNIT_ASSIGNED_CONTEXT((#8267,#8269,#8270))
REPRESENTATION_CONTEXT('','3D')
);
#8265=(
GEOMETRIC_REPRESENTATION_CONTEXT(3)
GLOBAL_UNCERTAINTY_ASSIGNED_CONTEXT((#8240))
GLOBAL_UNIT_ASSIGNED_CONTEXT((#8267,#8269,#8270))
REPRESENTATION_CONTEXT('','3D')
);
#8266=(
GEOMETRIC_REPRESENTATION_CONTEXT(3)
GLOBAL_UNCERTAINTY_ASSIGNED_CONTEXT((#8241))
GLOBAL_UNIT_ASSIGNED_CONTEXT((#8267,#8269,#8270))
REPRESENTATION_CONTEXT('','3D')
);
#8267=(
LENGTH_UNIT()
NAMED_UNIT(*)
SI_UNIT(.CENTI.,.METRE.)
);
#8268=(
LENGTH_UNIT()
NAMED_UNIT(*)
SI_UNIT($,.METRE.)
);
#8269=(
NAMED_UNIT(*)
PLANE_ANGLE_UNIT()
SI_UNIT($,.RADIAN.)
);
#8270=(
NAMED_UNIT(*)
SI_UNIT($,.STERADIAN.)
SOLID_ANGLE_UNIT()
);
#8271=SHAPE_DEFINITION_REPRESENTATION(#8295,#8358);
#8272=SHAPE_DEFINITION_REPRESENTATION(#8296,#8359);
#8273=SHAPE_DEFINITION_REPRESENTATION(#8297,#8360);
#8274=SHAPE_DEFINITION_REPRESENTATION(#8298,#8361);
#8275=SHAPE_DEFINITION_REPRESENTATION(#8299,#8362);
#8276=SHAPE_DEFINITION_REPRESENTATION(#8300,#8363);
#8277=SHAPE_DEFINITION_REPRESENTATION(#8301,#8364);
#8278=SHAPE_DEFINITION_REPRESENTATION(#8302,#8365);
#8279=SHAPE_DEFINITION_REPRESENTATION(#8303,#8366);
#8280=SHAPE_DEFINITION_REPRESENTATION(#8304,#8367);
#8281=SHAPE_DEFINITION_REPRESENTATION(#8305,#8368);
#8282=SHAPE_DEFINITION_REPRESENTATION(#8306,#8369);
#8283=SHAPE_DEFINITION_REPRESENTATION(#8307,#8370);
#8284=SHAPE_DEFINITION_REPRESENTATION(#8308,#8371);
#8285=SHAPE_DEFINITION_REPRESENTATION(#8309,#8372);
#8286=SHAPE_DEFINITION_REPRESENTATION(#8310,#8373);
#8287=SHAPE_DEFINITION_REPRESENTATION(#8311,#8374);
#8288=SHAPE_DEFINITION_REPRESENTATION(#8312,#8375);
#8289=SHAPE_DEFINITION_REPRESENTATION(#8313,#8376);
#8290=SHAPE_DEFINITION_REPRESENTATION(#8314,#8377);
#8291=SHAPE_DEFINITION_REPRESENTATION(#8315,#8378);
#8292=SHAPE_DEFINITION_REPRESENTATION(#8318,#8379);
#8293=SHAPE_DEFINITION_REPRESENTATION(#8319,#8380);
#8294=SHAPE_DEFINITION_REPRESENTATION(#8320,#8381);
#8295=PRODUCT_DEFINITION_SHAPE('',$,#8383);
#8296=PRODUCT_DEFINITION_SHAPE('',$,#8384);
#8297=PRODUCT_DEFINITION_SHAPE('',$,#8385);
#8298=PRODUCT_DEFINITION_SHAPE('',$,#8386);
#8299=PRODUCT_DEFINITION_SHAPE('',$,#8387);
#8300=PRODUCT_DEFINITION_SHAPE('',$,#8388);
#8301=PRODUCT_DEFINITION_SHAPE('',$,#8389);
#8302=PRODUCT_DEFINITION_SHAPE('',$,#8390);
#8303=PRODUCT_DEFINITION_SHAPE('',$,#8391);
#8304=PRODUCT_DEFINITION_SHAPE('',$,#8392);
#8305=PRODUCT_DEFINITION_SHAPE('',$,#8393);
#8306=PRODUCT_DEFINITION_SHAPE('',$,#8394);
#8307=PRODUCT_DEFINITION_SHAPE('',$,#8395);
#8308=PRODUCT_DEFINITION_SHAPE('',$,#8396);
#8309=PRODUCT_DEFINITION_SHAPE('',$,#8397);
#8310=PRODUCT_DEFINITION_SHAPE('',$,#8398);
#8311=PRODUCT_DEFINITION_SHAPE('',$,#8399);
#8312=PRODUCT_DEFINITION_SHAPE('',$,#8400);
#8313=PRODUCT_DEFINITION_SHAPE('',$,#8401);
#8314=PRODUCT_DEFINITION_SHAPE('',$,#8402);
#8315=PRODUCT_DEFINITION_SHAPE('',$,#8403);
#8316=PRODUCT_DEFINITION_SHAPE($,$,#128);
#8317=PRODUCT_DEFINITION_SHAPE($,$,#129);
#8318=PRODUCT_DEFINITION_SHAPE('',$,#8404);
#8319=PRODUCT_DEFINITION_SHAPE('',$,#8405);
#8320=PRODUCT_DEFINITION_SHAPE('',$,#8406);
#8321=PRODUCT_DEFINITION_SHAPE($,$,#130);
#8322=PRODUCT_DEFINITION_SHAPE($,$,#131);
#8323=PRODUCT_DEFINITION_SHAPE($,$,#132);
#8324=PRODUCT_DEFINITION_SHAPE($,$,#133);
#8325=PRODUCT_DEFINITION_SHAPE($,$,#134);
#8326=PRODUCT_DEFINITION_SHAPE($,$,#135);
#8327=PRODUCT_DEFINITION_SHAPE($,$,#136);
#8328=PRODUCT_DEFINITION_SHAPE($,$,#137);
#8329=PRODUCT_DEFINITION_SHAPE($,$,#138);
#8330=PRODUCT_DEFINITION_SHAPE($,$,#139);
#8331=PRODUCT_DEFINITION_SHAPE($,$,#140);
#8332=PRODUCT_DEFINITION_SHAPE($,$,#141);
#8333=PRODUCT_DEFINITION_SHAPE($,$,#142);
#8334=PRODUCT_DEFINITION_SHAPE($,$,#143);
#8335=PRODUCT_DEFINITION_SHAPE($,$,#144);
#8336=PRODUCT_DEFINITION_SHAPE($,$,#145);
#8337=PRODUCT_DEFINITION_SHAPE($,$,#146);
#8338=PRODUCT_DEFINITION_SHAPE($,$,#147);
#8339=PRODUCT_DEFINITION_SHAPE($,$,#148);
#8340=PRODUCT_DEFINITION_SHAPE($,$,#149);
#8341=PRODUCT_DEFINITION_SHAPE($,$,#150);
#8342=PRODUCT_DEFINITION_SHAPE($,$,#151);
#8343=PRODUCT_DEFINITION_SHAPE($,$,#152);
#8344=PRODUCT_DEFINITION_SHAPE($,$,#153);
#8345=PRODUCT_DEFINITION_SHAPE($,$,#154);
#8346=PRODUCT_DEFINITION_SHAPE($,$,#155);
#8347=PRODUCT_DEFINITION_SHAPE($,$,#156);
#8348=PRODUCT_DEFINITION_SHAPE($,$,#157);
#8349=PRODUCT_DEFINITION_SHAPE($,$,#158);
#8350=PRODUCT_DEFINITION_SHAPE($,$,#159);
#8351=PRODUCT_DEFINITION_SHAPE($,$,#160);
#8352=PRODUCT_DEFINITION_SHAPE($,$,#161);
#8353=PRODUCT_DEFINITION_SHAPE($,$,#162);
#8354=PRODUCT_DEFINITION_SHAPE($,$,#163);
#8355=PRODUCT_DEFINITION_SHAPE($,$,#164);
#8356=PRODUCT_DEFINITION_SHAPE($,$,#165);
#8357=PRODUCT_DEFINITION_SHAPE($,$,#166);
#8358=SHAPE_REPRESENTATION('',(#4849,#5345,#5346,#5347,#5348,#5349,#5350,
#5351,#5352,#5353,#5354,#5355,#5356,#5357,#5358,#5359,#5360,#5361,#5362,
#5363,#5364,#5365,#5366,#5367,#5368,#5369,#5370,#5371,#5372,#5373,#5374,
#5375,#5376,#5377,#5378,#5379,#5380,#5381),#8242);
#8359=SHAPE_REPRESENTATION('',(#4850),#8243);
#8360=SHAPE_REPRESENTATION('',(#4885),#8244);
#8361=SHAPE_REPRESENTATION('',(#4892),#8245);
#8362=SHAPE_REPRESENTATION('',(#4899),#8246);
#8363=SHAPE_REPRESENTATION('',(#4930),#8247);
#8364=SHAPE_REPRESENTATION('',(#4961),#8248);
#8365=SHAPE_REPRESENTATION('',(#5004),#8249);
#8366=SHAPE_REPRESENTATION('',(#5039),#8250);
#8367=SHAPE_REPRESENTATION('',(#5129),#8251);
#8368=SHAPE_REPRESENTATION('',(#5138),#8252);
#8369=SHAPE_REPRESENTATION('',(#5147),#8253);
#8370=SHAPE_REPRESENTATION('',(#5156),#8254);
#8371=SHAPE_REPRESENTATION('',(#5165),#8255);
#8372=SHAPE_REPRESENTATION('',(#5178),#8256);
#8373=SHAPE_REPRESENTATION('',(#5184),#8257);
#8374=SHAPE_REPRESENTATION('',(#5190),#8258);
#8375=SHAPE_REPRESENTATION('',(#5203),#8259);
#8376=SHAPE_REPRESENTATION('',(#5227,#5269,#5270),#8260);
#8377=SHAPE_REPRESENTATION('',(#5228),#8261);
#8378=SHAPE_REPRESENTATION('',(#5256),#8262);
#8379=SHAPE_REPRESENTATION('',(#5271),#8263);
#8380=SHAPE_REPRESENTATION('',(#5295),#8264);
#8381=SHAPE_REPRESENTATION('',(#5321),#8265);
#8382=PRODUCT_DEFINITION_CONTEXT('part definition',#8456,'design');
#8383=PRODUCT_DEFINITION('PAT-082','PAT-082',
#8407,#8382);
#8384=PRODUCT_DEFINITION('Base','Base',#8408,#8382);
#8385=PRODUCT_DEFINITION('Bonded pad','Bonded pad',#8409,#8382);
#8386=PRODUCT_DEFINITION('Bonded pad (1)','Bonded pad (1)',#8410,
#8382);
#8387=PRODUCT_DEFINITION('Mounting foot','Mounting foot',#8411,
#8382);
#8388=PRODUCT_DEFINITION('Mounting foot (1)','Mounting foot (1)',
#8412,#8382);
#8389=PRODUCT_DEFINITION('Service cover','Service cover',#8413,
#8382);
#8390=PRODUCT_DEFINITION('Cover gasket','Cover gasket',#8414,
#8382);
#8391=PRODUCT_DEFINITION('Manifold block','Manifold block',#8415,
#8382);
#8392=PRODUCT_DEFINITION('Outlet tube','Outlet tube',#8416,
#8382);
#8393=PRODUCT_DEFINITION('Outlet tube (1)','Outlet tube (1)',
#8417,#8382);
#8394=PRODUCT_DEFINITION('Outlet tube (2)','Outlet tube (2)',
#8418,#8382);
#8395=PRODUCT_DEFINITION('Outlet tube (3)','Outlet tube (3)',
#8419,#8382);
#8396=PRODUCT_DEFINITION('Blanking plug','Blanking plug',#8420,
#8382);
#8397=PRODUCT_DEFINITION('Cover locating dowel',
'Cover locating dowel',#8421,#8382);
#8398=PRODUCT_DEFINITION('Cover locating dowel (1)',
'Cover locating dowel (1)',#8422,#8382);
#8399=PRODUCT_DEFINITION('Port label plate','Port label plate',
#8423,#8382);
#8400=PRODUCT_DEFINITION('M5x14 Cap Screw','M5x14 Cap Screw',
#8424,#8382);
#8401=PRODUCT_DEFINITION('Push-In Tube Fitting - 6 mm Tube, 1-8 Inch Tapered Pipe Thread',
'Push-In Tube Fitting - 6 mm Tube, 1-8 Inch Tapered Pipe Thread',#8425,
#8382);
#8402=PRODUCT_DEFINITION('Body','Body',#8426,#8382);
#8403=PRODUCT_DEFINITION('Release collar','Release collar',#8427,
#8382);
#8404=PRODUCT_DEFINITION('Hex Pipe Nipple - 1-4 Inch Tapered Pipe Thread',
'Hex Pipe Nipple - 1-4 Inch Tapered Pipe Thread',#8428,#8382);
#8405=PRODUCT_DEFINITION('Cap Screw - M4x16',
'Cap Screw - M4x16',#8429,#8382);
#8406=PRODUCT_DEFINITION('M4x10 Cap Screw','M4x10 Cap Screw',
#8430,#8382);
#8407=PRODUCT_DEFINITION_FORMATION('',$,#8458);
#8408=PRODUCT_DEFINITION_FORMATION('',$,#8459);
#8409=PRODUCT_DEFINITION_FORMATION('',$,#8460);
#8410=PRODUCT_DEFINITION_FORMATION('',$,#8461);
#8411=PRODUCT_DEFINITION_FORMATION('',$,#8462);
#8412=PRODUCT_DEFINITION_FORMATION('',$,#8463);
#8413=PRODUCT_DEFINITION_FORMATION('',$,#8464);
#8414=PRODUCT_DEFINITION_FORMATION('',$,#8465);
#8415=PRODUCT_DEFINITION_FORMATION('',$,#8466);
#8416=PRODUCT_DEFINITION_FORMATION('',$,#8467);
#8417=PRODUCT_DEFINITION_FORMATION('',$,#8468);
#8418=PRODUCT_DEFINITION_FORMATION('',$,#8469);
#8419=PRODUCT_DEFINITION_FORMATION('',$,#8470);
#8420=PRODUCT_DEFINITION_FORMATION('',$,#8471);
#8421=PRODUCT_DEFINITION_FORMATION('',$,#8472);
#8422=PRODUCT_DEFINITION_FORMATION('',$,#8473);
#8423=PRODUCT_DEFINITION_FORMATION('',$,#8474);
#8424=PRODUCT_DEFINITION_FORMATION('',$,#8475);
#8425=PRODUCT_DEFINITION_FORMATION('',$,#8476);
#8426=PRODUCT_DEFINITION_FORMATION('',$,#8477);
#8427=PRODUCT_DEFINITION_FORMATION('',$,#8478);
#8428=PRODUCT_DEFINITION_FORMATION('',$,#8479);
#8429=PRODUCT_DEFINITION_FORMATION('',$,#8480);
#8430=PRODUCT_DEFINITION_FORMATION('',$,#8481);
#8431=PRODUCT_RELATED_PRODUCT_CATEGORY('PAT-082',
'PAT-082',(#8458));
#8432=PRODUCT_RELATED_PRODUCT_CATEGORY('Base','Base',(#8459));
#8433=PRODUCT_RELATED_PRODUCT_CATEGORY('Bonded pad','Bonded pad',(#8460));
#8434=PRODUCT_RELATED_PRODUCT_CATEGORY('Bonded pad (1)',
'Bonded pad (1)',(#8461));
#8435=PRODUCT_RELATED_PRODUCT_CATEGORY('Mounting foot','Mounting foot',
(#8462));
#8436=PRODUCT_RELATED_PRODUCT_CATEGORY('Mounting foot (1)',
'Mounting foot (1)',(#8463));
#8437=PRODUCT_RELATED_PRODUCT_CATEGORY('Service cover','Service cover',
(#8464));
#8438=PRODUCT_RELATED_PRODUCT_CATEGORY('Cover gasket','Cover gasket',(#8465));
#8439=PRODUCT_RELATED_PRODUCT_CATEGORY('Manifold block',
'Manifold block',(#8466));
#8440=PRODUCT_RELATED_PRODUCT_CATEGORY('Outlet tube','Outlet tube',(#8467));
#8441=PRODUCT_RELATED_PRODUCT_CATEGORY('Outlet tube (1)',
'Outlet tube (1)',(#8468));
#8442=PRODUCT_RELATED_PRODUCT_CATEGORY('Outlet tube (2)',
'Outlet tube (2)',(#8469));
#8443=PRODUCT_RELATED_PRODUCT_CATEGORY('Outlet tube (3)',
'Outlet tube (3)',(#8470));
#8444=PRODUCT_RELATED_PRODUCT_CATEGORY('Blanking plug','Blanking plug',
(#8471));
#8445=PRODUCT_RELATED_PRODUCT_CATEGORY('Cover locating dowel',
'Cover locating dowel',(#8472));
#8446=PRODUCT_RELATED_PRODUCT_CATEGORY('Cover locating dowel (1)',
'Cover locating dowel (1)',(#8473));
#8447=PRODUCT_RELATED_PRODUCT_CATEGORY('Port label plate',
'Port label plate',(#8474));
#8448=PRODUCT_RELATED_PRODUCT_CATEGORY('M5x14 Cap Screw',
'M5x14 Cap Screw',(#8475));
#8449=PRODUCT_RELATED_PRODUCT_CATEGORY(
'Push-In Tube Fitting - 6 mm Tube, 1-8 Inch Tapered Pipe Thread',
'Push-In Tube Fitting - 6 mm Tube, 1-8 Inch Tapered Pipe Thread',(#8476));
#8450=PRODUCT_RELATED_PRODUCT_CATEGORY('Body','Body',(#8477));
#8451=PRODUCT_RELATED_PRODUCT_CATEGORY('Release collar',
'Release collar',(#8478));
#8452=PRODUCT_RELATED_PRODUCT_CATEGORY(
'Hex Pipe Nipple - 1-4 Inch Tapered Pipe Thread',
'Hex Pipe Nipple - 1-4 Inch Tapered Pipe Thread',(#8479));
#8453=PRODUCT_RELATED_PRODUCT_CATEGORY('Cap Screw - M4x16',
'Cap Screw - M4x16',(#8480));
#8454=PRODUCT_RELATED_PRODUCT_CATEGORY('M4x10 Cap Screw',
'M4x10 Cap Screw',(#8481));
#8455=APPLICATION_PROTOCOL_DEFINITION('international standard',
'automotive_design',2009,#8456);
#8456=APPLICATION_CONTEXT(
'Core Data for Automotive Mechanical Design Process');
#8457=PRODUCT_CONTEXT('part definition',#8456,'mechanical');
#8458=PRODUCT('PAT-082','PAT-082',
'PAT-082',(#8457));
#8459=PRODUCT('Base','Base','Base',(#8457));
#8460=PRODUCT('Bonded pad','Bonded pad','Bonded pad',(#8457));
#8461=PRODUCT('Bonded pad (1)','Bonded pad (1)','Bonded pad (1)',
(#8457));
#8462=PRODUCT('Mounting foot','Mounting foot',
'Mounting foot',(#8457));
#8463=PRODUCT('Mounting foot (1)','Mounting foot (1)',
'Mounting foot (1)',(#8457));
#8464=PRODUCT('Service cover','Service cover',
'Service cover',(#8457));
#8465=PRODUCT('Cover gasket','Cover gasket','Cover gasket',
(#8457));
#8466=PRODUCT('Manifold block','Manifold block',
'Manifold block',(#8457));
#8467=PRODUCT('Outlet tube','Outlet tube','Outlet tube',(#8457));
#8468=PRODUCT('Outlet tube (1)','Outlet tube (1)',
'Outlet tube (1)',(#8457));
#8469=PRODUCT('Outlet tube (2)','Outlet tube (2)',
'Outlet tube (2)',(#8457));
#8470=PRODUCT('Outlet tube (3)','Outlet tube (3)',
'Outlet tube (3)',(#8457));
#8471=PRODUCT('Blanking plug','Blanking plug','Blanking plug',
(#8457));
#8472=PRODUCT('Cover locating dowel','Cover locating dowel',
'Cover locating dowel',(#8457));
#8473=PRODUCT('Cover locating dowel (1)','Cover locating dowel (1)',
'Cover locating dowel (1)',(#8457));
#8474=PRODUCT('Port label plate','Port label plate',
'Port label plate',(#8457));
#8475=PRODUCT('M5x14 Cap Screw','M5x14 Cap Screw',
'M5x14 Cap Screw',(#8457));
#8476=PRODUCT('Push-In Tube Fitting - 6 mm Tube, 1-8 Inch Tapered Pipe Thread',
'Push-In Tube Fitting - 6 mm Tube, 1-8 Inch Tapered Pipe Thread',
'Push-In Tube Fitting - 6 mm Tube, 1-8 Inch Tapered Pipe Thread',(#8457));
#8477=PRODUCT('Body','Body','Body',(#8457));
#8478=PRODUCT('Release collar','Release collar',
'Release collar',(#8457));
#8479=PRODUCT('Hex Pipe Nipple - 1-4 Inch Tapered Pipe Thread',
'Hex Pipe Nipple - 1-4 Inch Tapered Pipe Thread',
'Hex Pipe Nipple - 1-4 Inch Tapered Pipe Thread',(#8457));
#8480=PRODUCT('Cap Screw - M4x16','Cap Screw - M4x16',
'Cap Screw - M4x16',(#8457));
#8481=PRODUCT('M4x10 Cap Screw','M4x10 Cap Screw',
'M4x10 Cap Screw',(#8457));
#8482=PRESENTATION_STYLE_ASSIGNMENT((#8486));
#8483=PRESENTATION_STYLE_ASSIGNMENT((#8487));
#8484=PRESENTATION_STYLE_ASSIGNMENT((#8488));
#8485=PRESENTATION_STYLE_ASSIGNMENT((#8489));
#8486=SURFACE_STYLE_USAGE(.BOTH.,#8490);
#8487=SURFACE_STYLE_USAGE(.BOTH.,#8491);
#8488=SURFACE_STYLE_USAGE(.BOTH.,#8492);
#8489=SURFACE_STYLE_USAGE(.BOTH.,#8493);
#8490=SURFACE_SIDE_STYLE('',(#8494));
#8491=SURFACE_SIDE_STYLE('',(#8495));
#8492=SURFACE_SIDE_STYLE('',(#8496));
#8493=SURFACE_SIDE_STYLE('',(#8497));
#8494=SURFACE_STYLE_FILL_AREA(#8498);
#8495=SURFACE_STYLE_FILL_AREA(#8499);
#8496=SURFACE_STYLE_FILL_AREA(#8500);
#8497=SURFACE_STYLE_FILL_AREA(#8501);
#8498=FILL_AREA_STYLE('Steel - Satin',(#8502));
#8499=FILL_AREA_STYLE('CAD Library Painted - Deep blue',(#8503));
#8500=FILL_AREA_STYLE('CAD Library Painted - Graphite',(#8504));
#8501=FILL_AREA_STYLE('CAD Library Painted - Engineering blue',(#8505));
#8502=FILL_AREA_STYLE_COLOUR('Steel - Satin',#8506);
#8503=FILL_AREA_STYLE_COLOUR('CAD Library Painted - Deep blue',#8507);
#8504=FILL_AREA_STYLE_COLOUR('CAD Library Painted - Graphite',#8508);
#8505=FILL_AREA_STYLE_COLOUR('CAD Library Painted - Engineering blue',#8509);
#8506=COLOUR_RGB('Steel - Satin',0.627450980392157,0.627450980392157,0.627450980392157);
#8507=COLOUR_RGB('CAD Library Painted - Deep blue',0.0784313725490196,0.203921568627451,
0.349019607843137);
#8508=COLOUR_RGB('CAD Library Painted - Graphite',0.168627450980392,0.192156862745098,
0.231372549019608);
#8509=COLOUR_RGB('CAD Library Painted - Engineering blue',0.12156862745098,
0.356862745098039,0.6);
#8510=COLOUR_RGB('Dark Blue',0.08,0.2,0.34);
#8511=FILL_AREA_STYLE_COLOUR('',#8510);
#8512=FILL_AREA_STYLE('',(#8511));
#8513=SURFACE_STYLE_FILL_AREA(#8512);
#8514=SURFACE_SIDE_STYLE('',(#8513));
#8515=SURFACE_STYLE_USAGE(.BOTH.,#8514);
#8516=PRESENTATION_STYLE_ASSIGNMENT((#8515));
#8517=COLOUR_RGB('Light Blue',0.38,0.62,0.78);
#8518=FILL_AREA_STYLE_COLOUR('',#8517);
#8519=FILL_AREA_STYLE('',(#8518));
#8520=SURFACE_STYLE_FILL_AREA(#8519);
#8521=SURFACE_SIDE_STYLE('',(#8520));
#8522=SURFACE_STYLE_USAGE(.BOTH.,#8521);
#8523=PRESENTATION_STYLE_ASSIGNMENT((#8522));
#8524=COLOUR_RGB('Sky Blue',0.24,0.69,0.87);
#8525=FILL_AREA_STYLE_COLOUR('',#8524);
#8526=FILL_AREA_STYLE('',(#8525));
#8527=SURFACE_STYLE_FILL_AREA(#8526);
#8528=SURFACE_SIDE_STYLE('',(#8527));
#8529=SURFACE_STYLE_USAGE(.BOTH.,#8528);
#8530=PRESENTATION_STYLE_ASSIGNMENT((#8529));
#8531=COLOUR_RGB('Grey',0.48,0.52,0.57);
#8532=FILL_AREA_STYLE_COLOUR('',#8531);
#8533=FILL_AREA_STYLE('',(#8532));
#8534=SURFACE_STYLE_FILL_AREA(#8533);
#8535=SURFACE_SIDE_STYLE('',(#8534));
#8536=SURFACE_STYLE_USAGE(.BOTH.,#8535);
#8537=PRESENTATION_STYLE_ASSIGNMENT((#8536));
#8538=COLOUR_RGB('Black',0.12,0.14,0.17);
#8539=FILL_AREA_STYLE_COLOUR('',#8538);
#8540=FILL_AREA_STYLE('',(#8539));
#8541=SURFACE_STYLE_FILL_AREA(#8540);
#8542=SURFACE_SIDE_STYLE('',(#8541));
#8543=SURFACE_STYLE_USAGE(.BOTH.,#8542);
#8544=PRESENTATION_STYLE_ASSIGNMENT((#8543));
#8545=COLOUR_RGB('Off White',0.89,0.88,0.83);
#8546=FILL_AREA_STYLE_COLOUR('',#8545);
#8547=FILL_AREA_STYLE('',(#8546));
#8548=SURFACE_STYLE_FILL_AREA(#8547);
#8549=SURFACE_SIDE_STYLE('',(#8548));
#8550=SURFACE_STYLE_USAGE(.BOTH.,#8549);
#8551=PRESENTATION_STYLE_ASSIGNMENT((#8550));
ENDSEC;
END-ISO-10303-21;
